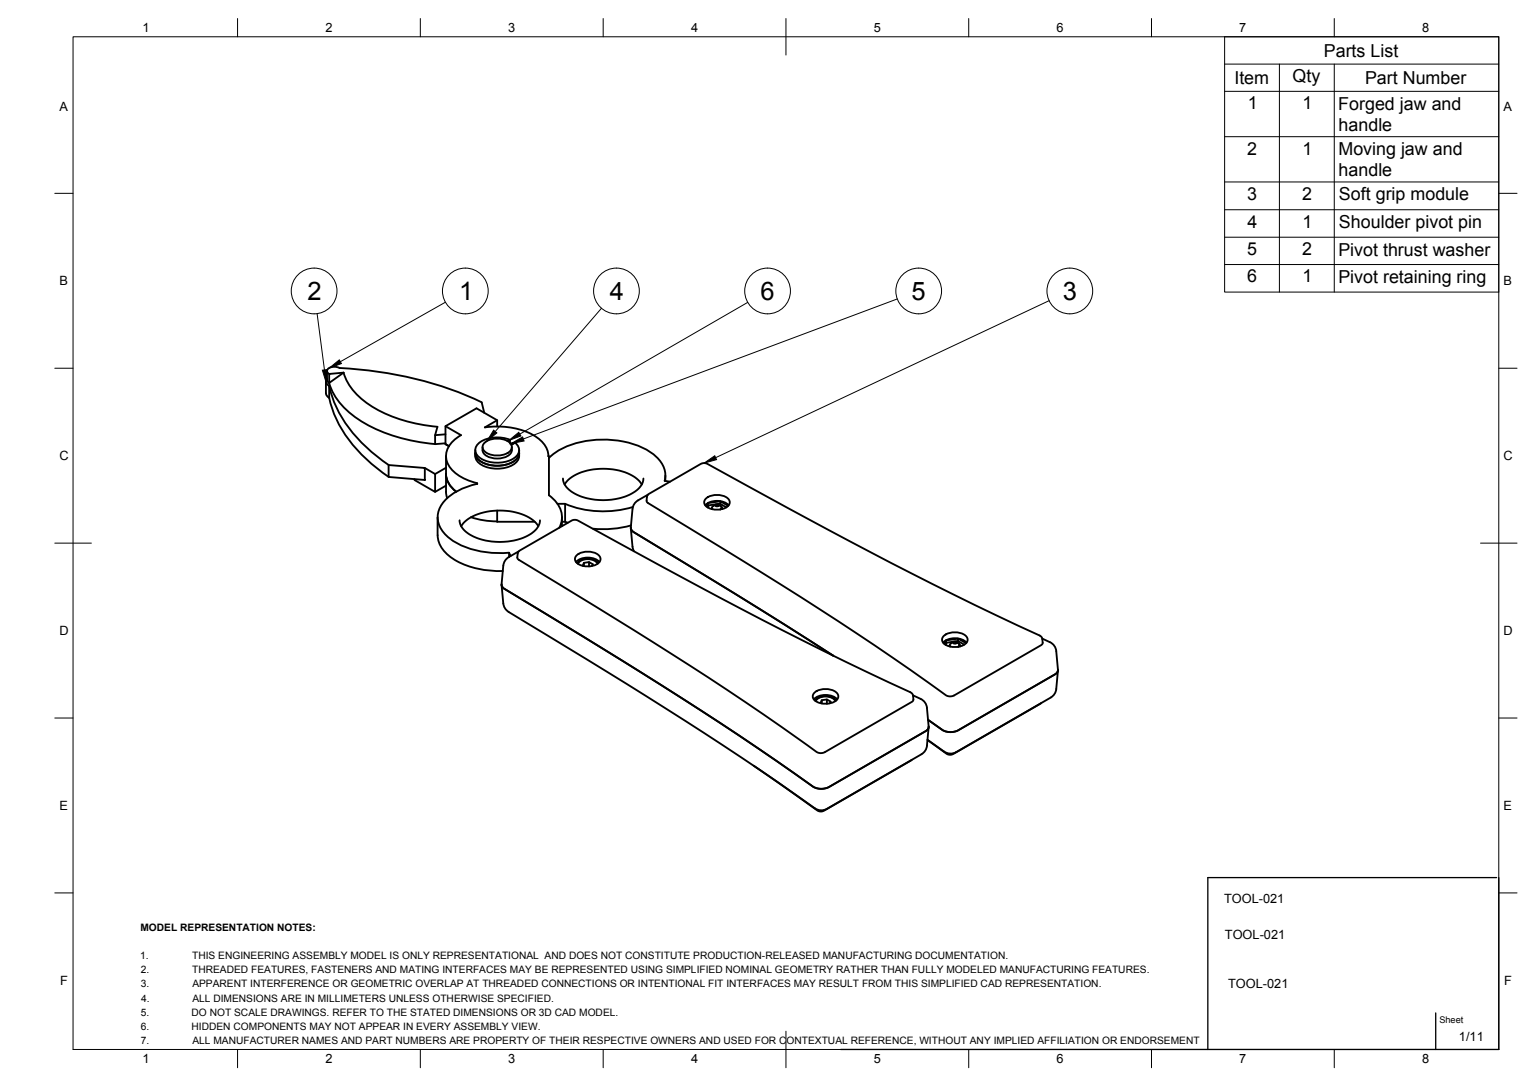
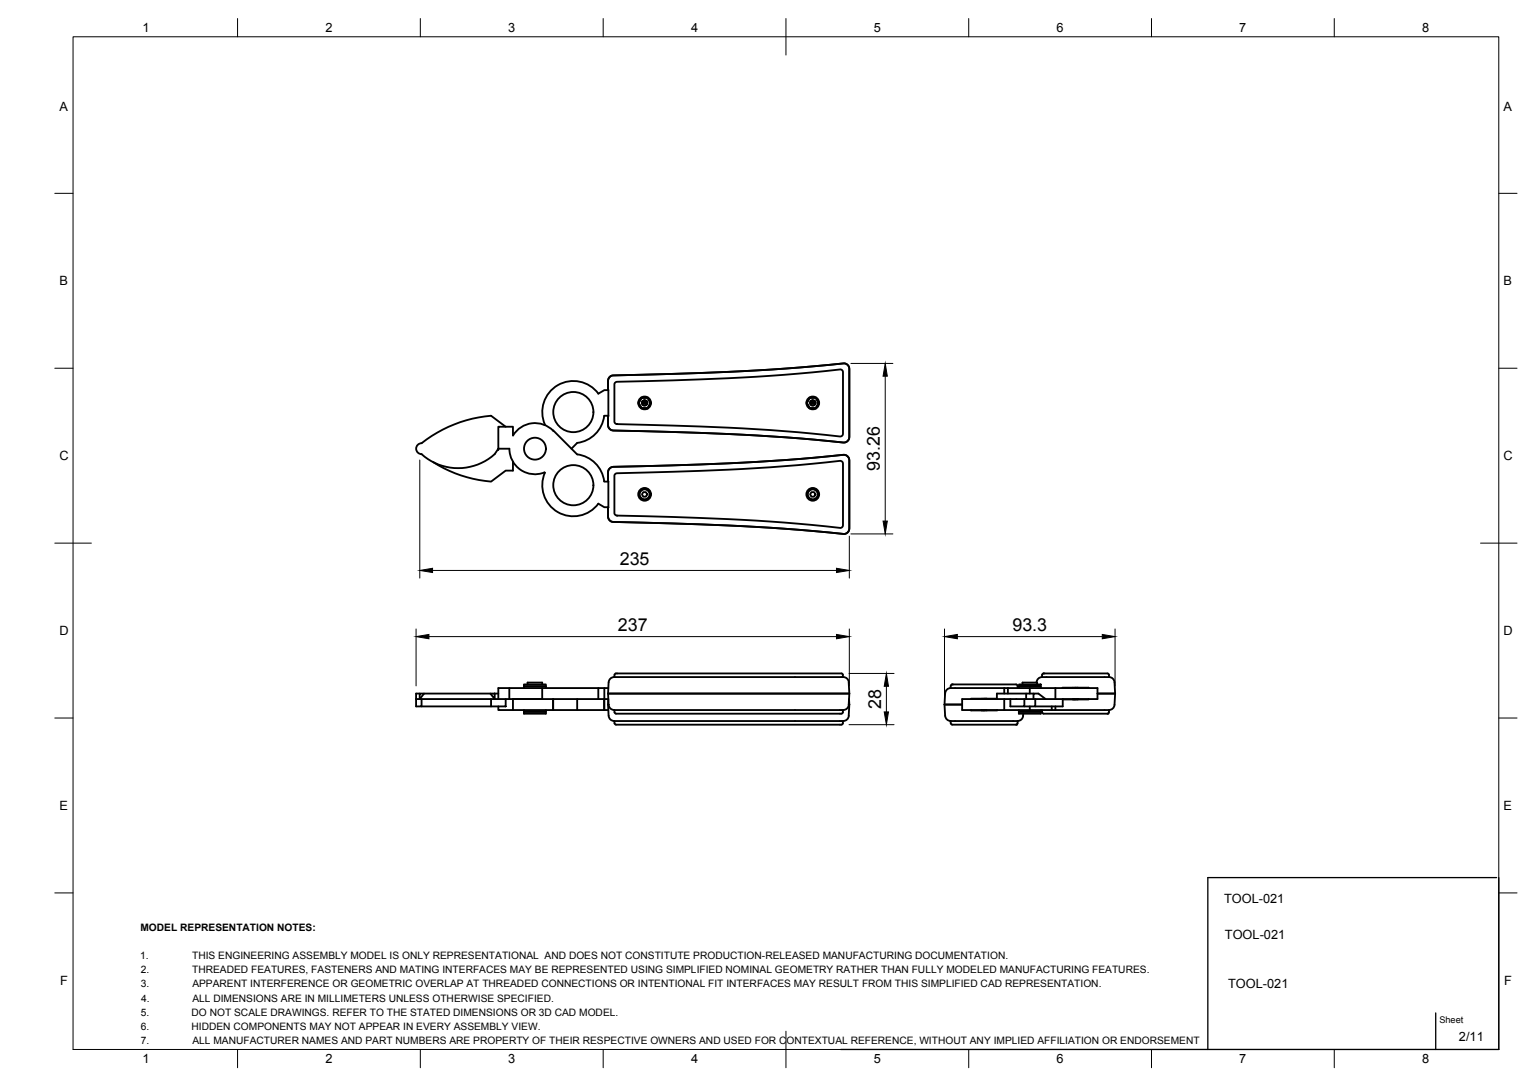
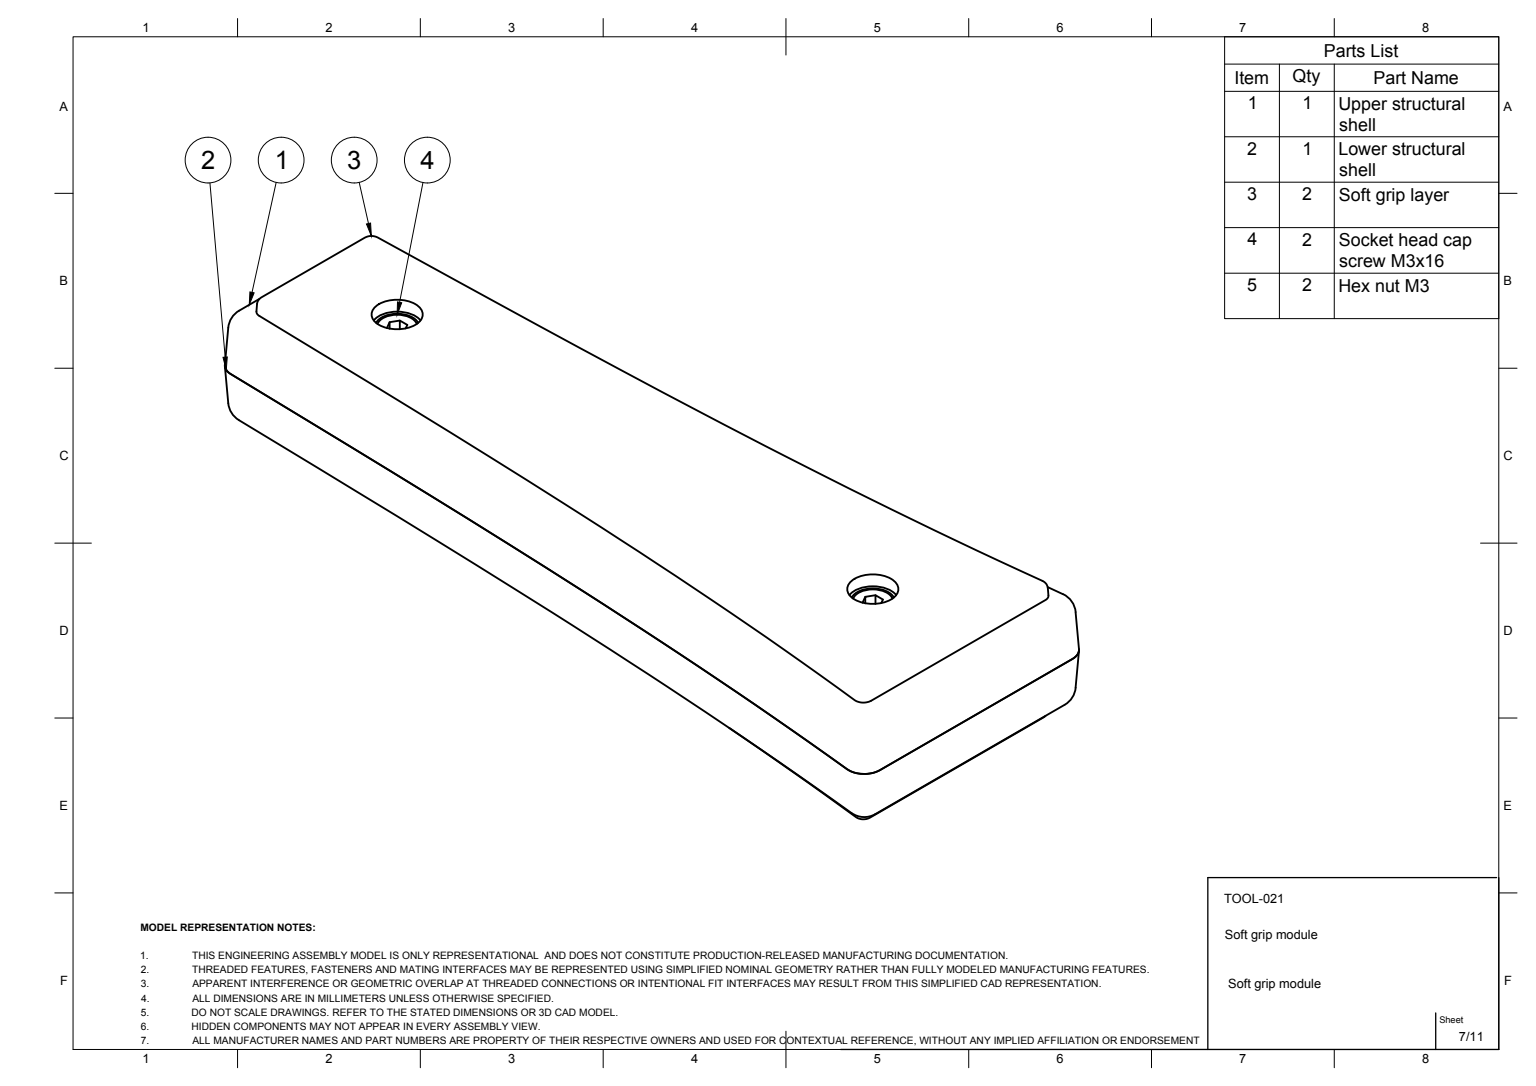
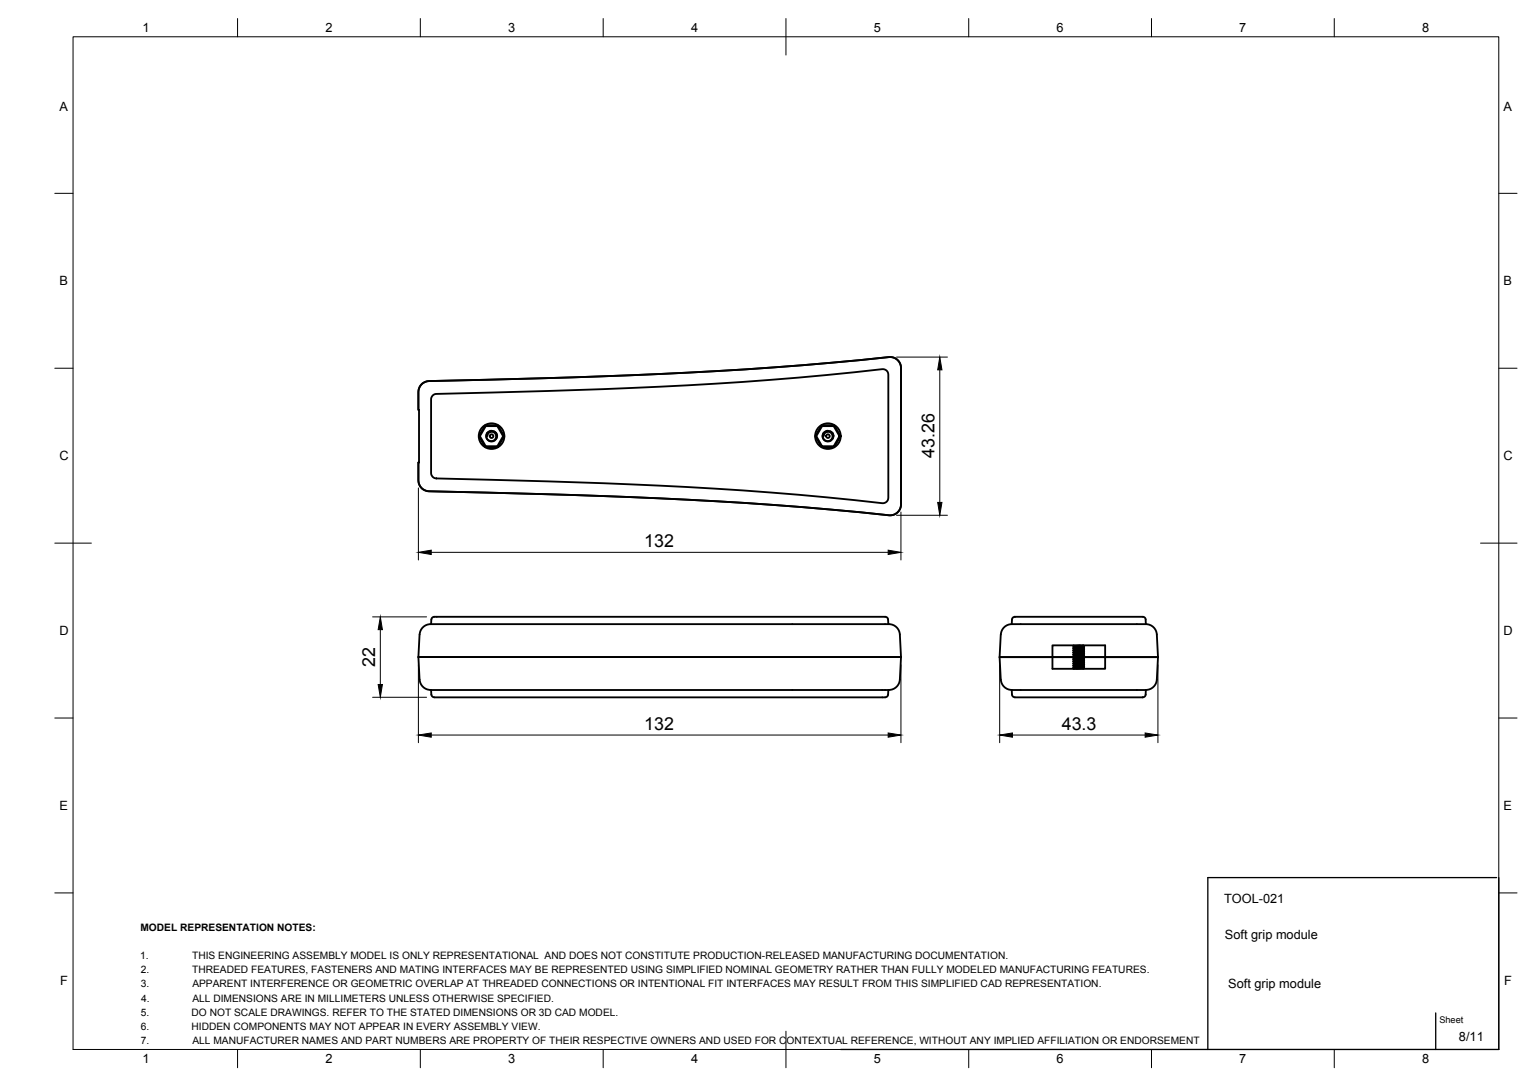
ISO-10303-21;
HEADER;
/* Generated by software containing ST-Developer
 * from STEP Tools, Inc. (www.steptools.com) 
 */

FILE_DESCRIPTION(
/* description */ (''),
/* implementation_level */ '2;1');

FILE_NAME(
/* name */ 'TOOL-021.step',
/* time_stamp */ '2026-11-10T09:05:57-08:00',
/* author */ (''),
/* organization */ (''),
/* preprocessor_version */ 'ST-DEVELOPER v20.2',
/* originating_system */ 'Autodesk Translation Framework v15.17.0.0',
/* authorisation */ '');

FILE_SCHEMA (('AUTOMOTIVE_DESIGN { 1 0 10303 214 3 1 1 }'));
ENDSEC;

DATA;
#10=MECHANICAL_DESIGN_GEOMETRIC_PRESENTATION_REPRESENTATION('',(#565,#566,
#567,#568,#569,#570,#571,#572,#573,#574),#19618);
#11=ITEM_DEFINED_TRANSFORMATION($,$,#7373,#7744);
#12=ITEM_DEFINED_TRANSFORMATION($,$,#7475,#7745);
#13=ITEM_DEFINED_TRANSFORMATION($,$,#7583,#7746);
#14=ITEM_DEFINED_TRANSFORMATION($,$,#7636,#7747);
#15=ITEM_DEFINED_TRANSFORMATION($,$,#7718,#7748);
#16=ITEM_DEFINED_TRANSFORMATION($,$,#7583,#7749);
#17=ITEM_DEFINED_TRANSFORMATION($,$,#7636,#7750);
#18=ITEM_DEFINED_TRANSFORMATION($,$,#7718,#7751);
#19=ITEM_DEFINED_TRANSFORMATION($,$,#7225,#7761);
#20=ITEM_DEFINED_TRANSFORMATION($,$,#7285,#7762);
#21=ITEM_DEFINED_TRANSFORMATION($,$,#7372,#7763);
#22=ITEM_DEFINED_TRANSFORMATION($,$,#7343,#7764);
#23=ITEM_DEFINED_TRANSFORMATION($,$,#7752,#7765);
#24=ITEM_DEFINED_TRANSFORMATION($,$,#7361,#7766);
#25=ITEM_DEFINED_TRANSFORMATION($,$,#7372,#7767);
#26=ITEM_DEFINED_TRANSFORMATION($,$,#7752,#7768);
#27=(
REPRESENTATION_RELATIONSHIP($,$,#19669,#19668)
REPRESENTATION_RELATIONSHIP_WITH_TRANSFORMATION(#11)
SHAPE_REPRESENTATION_RELATIONSHIP()
);
#28=(
REPRESENTATION_RELATIONSHIP($,$,#19670,#19668)
REPRESENTATION_RELATIONSHIP_WITH_TRANSFORMATION(#12)
SHAPE_REPRESENTATION_RELATIONSHIP()
);
#29=(
REPRESENTATION_RELATIONSHIP($,$,#19671,#19668)
REPRESENTATION_RELATIONSHIP_WITH_TRANSFORMATION(#13)
SHAPE_REPRESENTATION_RELATIONSHIP()
);
#30=(
REPRESENTATION_RELATIONSHIP($,$,#19672,#19668)
REPRESENTATION_RELATIONSHIP_WITH_TRANSFORMATION(#14)
SHAPE_REPRESENTATION_RELATIONSHIP()
);
#31=(
REPRESENTATION_RELATIONSHIP($,$,#19673,#19668)
REPRESENTATION_RELATIONSHIP_WITH_TRANSFORMATION(#15)
SHAPE_REPRESENTATION_RELATIONSHIP()
);
#32=(
REPRESENTATION_RELATIONSHIP($,$,#19671,#19668)
REPRESENTATION_RELATIONSHIP_WITH_TRANSFORMATION(#16)
SHAPE_REPRESENTATION_RELATIONSHIP()
);
#33=(
REPRESENTATION_RELATIONSHIP($,$,#19672,#19668)
REPRESENTATION_RELATIONSHIP_WITH_TRANSFORMATION(#17)
SHAPE_REPRESENTATION_RELATIONSHIP()
);
#34=(
REPRESENTATION_RELATIONSHIP($,$,#19673,#19668)
REPRESENTATION_RELATIONSHIP_WITH_TRANSFORMATION(#18)
SHAPE_REPRESENTATION_RELATIONSHIP()
);
#35=(
REPRESENTATION_RELATIONSHIP($,$,#19664,#19663)
REPRESENTATION_RELATIONSHIP_WITH_TRANSFORMATION(#19)
SHAPE_REPRESENTATION_RELATIONSHIP()
);
#36=(
REPRESENTATION_RELATIONSHIP($,$,#19665,#19663)
REPRESENTATION_RELATIONSHIP_WITH_TRANSFORMATION(#20)
SHAPE_REPRESENTATION_RELATIONSHIP()
);
#37=(
REPRESENTATION_RELATIONSHIP($,$,#19668,#19663)
REPRESENTATION_RELATIONSHIP_WITH_TRANSFORMATION(#21)
SHAPE_REPRESENTATION_RELATIONSHIP()
);
#38=(
REPRESENTATION_RELATIONSHIP($,$,#19666,#19663)
REPRESENTATION_RELATIONSHIP_WITH_TRANSFORMATION(#22)
SHAPE_REPRESENTATION_RELATIONSHIP()
);
#39=(
REPRESENTATION_RELATIONSHIP($,$,#19674,#19663)
REPRESENTATION_RELATIONSHIP_WITH_TRANSFORMATION(#23)
SHAPE_REPRESENTATION_RELATIONSHIP()
);
#40=(
REPRESENTATION_RELATIONSHIP($,$,#19667,#19663)
REPRESENTATION_RELATIONSHIP_WITH_TRANSFORMATION(#24)
SHAPE_REPRESENTATION_RELATIONSHIP()
);
#41=(
REPRESENTATION_RELATIONSHIP($,$,#19668,#19663)
REPRESENTATION_RELATIONSHIP_WITH_TRANSFORMATION(#25)
SHAPE_REPRESENTATION_RELATIONSHIP()
);
#42=(
REPRESENTATION_RELATIONSHIP($,$,#19674,#19663)
REPRESENTATION_RELATIONSHIP_WITH_TRANSFORMATION(#26)
SHAPE_REPRESENTATION_RELATIONSHIP()
);
#43=CONTEXT_DEPENDENT_SHAPE_REPRESENTATION(#27,#19646);
#44=CONTEXT_DEPENDENT_SHAPE_REPRESENTATION(#28,#19647);
#45=CONTEXT_DEPENDENT_SHAPE_REPRESENTATION(#29,#19648);
#46=CONTEXT_DEPENDENT_SHAPE_REPRESENTATION(#30,#19649);
#47=CONTEXT_DEPENDENT_SHAPE_REPRESENTATION(#31,#19650);
#48=CONTEXT_DEPENDENT_SHAPE_REPRESENTATION(#32,#19651);
#49=CONTEXT_DEPENDENT_SHAPE_REPRESENTATION(#33,#19652);
#50=CONTEXT_DEPENDENT_SHAPE_REPRESENTATION(#34,#19653);
#51=CONTEXT_DEPENDENT_SHAPE_REPRESENTATION(#35,#19655);
#52=CONTEXT_DEPENDENT_SHAPE_REPRESENTATION(#36,#19656);
#53=CONTEXT_DEPENDENT_SHAPE_REPRESENTATION(#37,#19657);
#54=CONTEXT_DEPENDENT_SHAPE_REPRESENTATION(#38,#19658);
#55=CONTEXT_DEPENDENT_SHAPE_REPRESENTATION(#39,#19659);
#56=CONTEXT_DEPENDENT_SHAPE_REPRESENTATION(#40,#19660);
#57=CONTEXT_DEPENDENT_SHAPE_REPRESENTATION(#41,#19661);
#58=CONTEXT_DEPENDENT_SHAPE_REPRESENTATION(#42,#19662);
#59=NEXT_ASSEMBLY_USAGE_OCCURRENCE('Upper structural shell:1',
'Upper structural shell:1','Upper structural shell:1',#19681,#19682,
'Upper structural shell:1');
#60=NEXT_ASSEMBLY_USAGE_OCCURRENCE('Lower structural shell:1',
'Lower structural shell:1','Lower structural shell:1',#19681,#19683,
'Lower structural shell:1');
#61=NEXT_ASSEMBLY_USAGE_OCCURRENCE('Soft grip layer:1',
'Soft grip layer:1','Soft grip layer:1',#19681,#19684,
'Soft grip layer:1');
#62=NEXT_ASSEMBLY_USAGE_OCCURRENCE('Socket head cap screw M3x16:1',
'Socket head cap screw M3x16:1','Socket head cap screw M3x16:1',#19681,
#19685,'Socket head cap screw M3x16:1');
#63=NEXT_ASSEMBLY_USAGE_OCCURRENCE('Hex nut M3:1','Hex nut M3:1',
'Hex nut M3:1',#19681,#19686,'Hex nut M3:1');
#64=NEXT_ASSEMBLY_USAGE_OCCURRENCE('Soft grip layer:2',
'Soft grip layer:2','Soft grip layer:2',#19681,#19684,
'Soft grip layer:2');
#65=NEXT_ASSEMBLY_USAGE_OCCURRENCE('Socket head cap screw M3x16:2',
'Socket head cap screw M3x16:2','Socket head cap screw M3x16:2',#19681,
#19685,'Socket head cap screw M3x16:2');
#66=NEXT_ASSEMBLY_USAGE_OCCURRENCE('Hex nut M3:2','Hex nut M3:2',
'Hex nut M3:2',#19681,#19686,'Hex nut M3:2');
#67=NEXT_ASSEMBLY_USAGE_OCCURRENCE('Forged jaw and handle:1',
'Forged jaw and handle:1','Forged jaw and handle:1',#19676,#19677,
'Forged jaw and handle:1');
#68=NEXT_ASSEMBLY_USAGE_OCCURRENCE('Moving jaw and handle:1',
'Moving jaw and handle:1','Moving jaw and handle:1',#19676,#19678,
'Moving jaw and handle:1');
#69=NEXT_ASSEMBLY_USAGE_OCCURRENCE('Soft grip module:1',
'Soft grip module:1','Soft grip module:1',#19676,#19681,
'Soft grip module:1');
#70=NEXT_ASSEMBLY_USAGE_OCCURRENCE('Shoulder pivot pin:1',
'Shoulder pivot pin:1','Shoulder pivot pin:1',#19676,#19679,
'Shoulder pivot pin:1');
#71=NEXT_ASSEMBLY_USAGE_OCCURRENCE('Pivot thrust washer:1',
'Pivot thrust washer:1','Pivot thrust washer:1',#19676,#19687,
'Pivot thrust washer:1');
#72=NEXT_ASSEMBLY_USAGE_OCCURRENCE('Pivot retaining ring:1',
'Pivot retaining ring:1','Pivot retaining ring:1',#19676,#19680,
'Pivot retaining ring:1');
#73=NEXT_ASSEMBLY_USAGE_OCCURRENCE('Soft grip module:2',
'Soft grip module:2','Soft grip module:2',#19676,#19681,
'Soft grip module:2');
#74=NEXT_ASSEMBLY_USAGE_OCCURRENCE('Pivot thrust washer:2',
'Pivot thrust washer:2','Pivot thrust washer:2',#19676,#19687,
'Pivot thrust washer:2');
#75=SPHERICAL_SURFACE('',#7438,0.0999999999999999);
#76=SPHERICAL_SURFACE('',#7441,0.0999999999999997);
#77=SPHERICAL_SURFACE('',#7445,0.0999999999999998);
#78=SPHERICAL_SURFACE('',#7449,0.1);
#79=SPHERICAL_SURFACE('',#7454,0.3);
#80=SPHERICAL_SURFACE('',#7458,0.3);
#81=SPHERICAL_SURFACE('',#7462,0.3);
#82=SPHERICAL_SURFACE('',#7467,0.3);
#83=SPHERICAL_SURFACE('',#7546,0.0999999999999999);
#84=SPHERICAL_SURFACE('',#7549,0.0999999999999997);
#85=SPHERICAL_SURFACE('',#7553,0.0999999999999998);
#86=SPHERICAL_SURFACE('',#7557,0.1);
#87=SPHERICAL_SURFACE('',#7562,0.3);
#88=SPHERICAL_SURFACE('',#7566,0.3);
#89=SPHERICAL_SURFACE('',#7570,0.3);
#90=SPHERICAL_SURFACE('',#7575,0.3);
#91=B_SPLINE_SURFACE_WITH_KNOTS('',3,3,((#10711,#10712,#10713,#10714),(#10715,
#10716,#10717,#10718),(#10719,#10720,#10721,#10722),(#10723,#10724,#10725,
#10726)),.UNSPECIFIED.,.F.,.F.,.F.,(4,4),(4,4),(0.0600191787356395,0.326709122771036),
(0.0105314009467253,0.683686938235975),.UNSPECIFIED.);
#92=B_SPLINE_SURFACE_WITH_KNOTS('',3,3,((#10731,#10732,#10733,#10734),(#10735,
#10736,#10737,#10738),(#10739,#10740,#10741,#10742),(#10743,#10744,#10745,
#10746)),.UNSPECIFIED.,.F.,.F.,.F.,(4,4),(4,4),(0.0251675824878611,0.0470055662028096),
(0.0103663370325175,0.682341693918943),.UNSPECIFIED.);
#93=B_SPLINE_SURFACE_WITH_KNOTS('',3,3,((#10756,#10757,#10758,#10759),(#10760,
#10761,#10762,#10763),(#10764,#10765,#10766,#10767),(#10768,#10769,#10770,
#10771),(#10772,#10773,#10774,#10775)),.UNSPECIFIED.,.F.,.F.,.F.,(4,1,4),
(4,4),(0.,0.571428571428571,1.),(0.796205213256333,4.31873271634551),
 .UNSPECIFIED.);
#94=B_SPLINE_SURFACE_WITH_KNOTS('',3,3,((#10780,#10781,#10782,#10783),(#10784,
#10785,#10786,#10787),(#10788,#10789,#10790,#10791),(#10792,#10793,#10794,
#10795),(#10796,#10797,#10798,#10799)),.UNSPECIFIED.,.F.,.F.,.F.,(4,1,4),
(4,4),(0.,0.571428571428571,1.),(0.335767855111383,0.605460332260614),
 .UNSPECIFIED.);
#95=B_SPLINE_SURFACE_WITH_KNOTS('',3,3,((#10818,#10819,#10820,#10821),(#10822,
#10823,#10824,#10825),(#10826,#10827,#10828,#10829),(#10830,#10831,#10832,
#10833),(#10834,#10835,#10836,#10837)),.UNSPECIFIED.,.F.,.F.,.F.,(4,1,4),
(4,4),(0.,0.571428571428571,1.),(8.8675541747208,12.3900816778099),
 .UNSPECIFIED.);
#96=B_SPLINE_SURFACE_WITH_KNOTS('',3,3,((#10842,#10843,#10844,#10845),(#10846,
#10847,#10848,#10849),(#10850,#10851,#10852,#10853),(#10854,#10855,#10856,
#10857)),.UNSPECIFIED.,.F.,.F.,.F.,(4,4),(4,4),(0.673290877228964,0.939980821264432),
(0.010531400969624,0.683686938235975),.UNSPECIFIED.);
#97=B_SPLINE_SURFACE_WITH_KNOTS('',3,3,((#10858,#10859,#10860,#10861),(#10862,
#10863,#10864,#10865),(#10866,#10867,#10868,#10869),(#10870,#10871,#10872,
#10873)),.UNSPECIFIED.,.F.,.F.,.F.,(4,4),(4,4),(0.952994433797115,0.974832417512139),
(0.0103663370325174,0.682341693895801),.UNSPECIFIED.);
#98=B_SPLINE_SURFACE_WITH_KNOTS('',3,3,((#10957,#10958,#10959,#10960),(#10961,
#10962,#10963,#10964),(#10965,#10966,#10967,#10968),(#10969,#10970,#10971,
#10972)),.UNSPECIFIED.,.F.,.F.,.F.,(4,4),(4,4),(0.341076481775573,0.660379921919131),
(0.0113804342297301,0.684288445414502),.UNSPECIFIED.);
#99=B_SPLINE_SURFACE_WITH_KNOTS('',3,3,((#10977,#10978,#10979,#10980),(#10981,
#10982,#10983,#10984),(#10985,#10986,#10987,#10988),(#10989,#10990,#10991,
#10992),(#10993,#10994,#10995,#10996)),.UNSPECIFIED.,.F.,.F.,.F.,(4,1,4),
(4,4),(0.,0.571428571428571,1.),(4.5128966022766,8.72381854299666),
 .UNSPECIFIED.);
#100=B_SPLINE_SURFACE_WITH_KNOTS('',3,3,((#11006,#11007,#11008,#11009),
(#11010,#11011,#11012,#11013),(#11014,#11015,#11016,#11017),(#11018,#11019,
#11020,#11021),(#11022,#11023,#11024,#11025)),.UNSPECIFIED.,.F.,.F.,.F.,
(4,1,4),(4,4),(0.,0.571428571428571,1.),(4.46246834806959,8.67339028878965),
 .UNSPECIFIED.);
#101=B_SPLINE_SURFACE_WITH_KNOTS('',3,3,((#11030,#11031,#11032,#11033),
(#11034,#11035,#11036,#11037),(#11038,#11039,#11040,#11041),(#11042,#11043,
#11044,#11045)),.UNSPECIFIED.,.F.,.F.,.F.,(4,4),(4,4),(0.33962007808087,
0.658923518224427),(0.0113804342297301,0.68428844541339),.UNSPECIFIED.);
#102=B_SPLINE_SURFACE_WITH_KNOTS('',3,3,((#11117,#11118,#11119,#11120),
(#11121,#11122,#11123,#11124),(#11125,#11126,#11127,#11128),(#11129,#11130,
#11131,#11132)),.UNSPECIFIED.,.F.,.F.,.F.,(4,4),(4,4),(0.67474627241906,
0.91907102854965),(0.0117551961069005,0.684448842095107),.UNSPECIFIED.);
#103=B_SPLINE_SURFACE_WITH_KNOTS('',3,3,((#11137,#11138,#11139,#11140),
(#11141,#11142,#11143,#11144),(#11145,#11146,#11147,#11148),(#11149,#11150,
#11151,#11152),(#11153,#11154,#11155,#11156)),.UNSPECIFIED.,.F.,.F.,.F.,
(4,1,4),(4,4),(0.,0.571428571428571,1.),(8.92068531110742,12.1251256661408),
 .UNSPECIFIED.);
#104=B_SPLINE_SURFACE_WITH_KNOTS('',3,3,((#11157,#11158,#11159,#11160),
(#11161,#11162,#11163,#11164),(#11165,#11166,#11167,#11168),(#11169,#11170,
#11171,#11172),(#11173,#11174,#11175,#11176)),.UNSPECIFIED.,.F.,.F.,.F.,
(4,1,4),(4,4),(0.,0.571428571428571,1.),(1.06116122492545,4.26560157995882),
 .UNSPECIFIED.);
#105=B_SPLINE_SURFACE_WITH_KNOTS('',3,3,((#11181,#11182,#11183,#11184),
(#11185,#11186,#11187,#11188),(#11189,#11190,#11191,#11192),(#11193,#11194,
#11195,#11196)),.UNSPECIFIED.,.F.,.F.,.F.,(4,4),(4,4),(0.0809289714503497,
0.325253727580939),(0.011755196108102,0.684448842095106),.UNSPECIFIED.);
#106=B_SPLINE_SURFACE_WITH_KNOTS('',3,3,((#11271,#11272,#11273,#11274),
(#11275,#11276,#11277,#11278),(#11279,#11280,#11281,#11282),(#11283,#11284,
#11285,#11286)),.UNSPECIFIED.,.F.,.F.,.F.,(4,4),(4,4),(0.932204931312898,
0.977820042778932),(0.0118590921259657,0.68448768567755),.UNSPECIFIED.);
#107=B_SPLINE_SURFACE_WITH_KNOTS('',3,3,((#11296,#11297,#11298,#11299),
(#11300,#11301,#11302,#11303),(#11304,#11305,#11306,#11307),(#11308,#11309,
#11310,#11311),(#11312,#11313,#11314,#11315)),.UNSPECIFIED.,.F.,.F.,.F.,
(4,1,4),(4,4),(0.,0.571428571428571,1.),(12.3228618033436,12.893479658151),
 .UNSPECIFIED.);
#108=B_SPLINE_SURFACE_WITH_KNOTS('',3,3,((#11329,#11330,#11331,#11332),
(#11333,#11334,#11335,#11336),(#11337,#11338,#11339,#11340),(#11341,#11342,
#11343,#11344)),.UNSPECIFIED.,.F.,.F.,.F.,(4,4),(4,4),(0.0221799572210682,
0.0677950686870383),(0.0118590921467069,0.68448768567755),.UNSPECIFIED.);
#109=B_SPLINE_SURFACE_WITH_KNOTS('',3,3,((#11354,#11355,#11356,#11357),
(#11358,#11359,#11360,#11361),(#11362,#11363,#11364,#11365),(#11366,#11367,
#11368,#11369),(#11370,#11371,#11372,#11373)),.UNSPECIFIED.,.F.,.F.,.F.,
(4,1,4),(4,4),(0.,0.571428571428571,1.),(0.29280723291527,0.863425087722636),
 .UNSPECIFIED.);
#110=B_SPLINE_SURFACE_WITH_KNOTS('',3,3,((#11387,#11388,#11389,#11390),
(#11391,#11392,#11393,#11394),(#11395,#11396,#11397,#11398),(#11399,#11400,
#11401,#11402),(#11403,#11404,#11405,#11406)),.UNSPECIFIED.,.F.,.F.,.F.,
(4,1,4),(4,4),(0.,0.571428571428571,1.),(0.00866835330220971,0.617725317592517),
 .UNSPECIFIED.);
#111=B_SPLINE_SURFACE_WITH_KNOTS('',3,3,((#11413,#11414,#11415,#11416),
(#11417,#11418,#11419,#11420),(#11421,#11422,#11423,#11424),(#11425,#11426,
#11427,#11428),(#11429,#11430,#11431,#11432),(#11433,#11434,#11435,#11436)),
 .UNSPECIFIED.,.F.,.F.,.F.,(4,1,1,4),(4,4),(0.,0.285714285714286,0.571428571428571,
1.),(0.00654045782928703,0.615688454110788),.UNSPECIFIED.);
#112=B_SPLINE_SURFACE_WITH_KNOTS('',3,3,((#11441,#11442,#11443,#11444),
(#11445,#11446,#11447,#11448),(#11449,#11450,#11451,#11452),(#11453,#11454,
#11455,#11456),(#11457,#11458,#11459,#11460),(#11461,#11462,#11463,#11464)),
 .UNSPECIFIED.,.F.,.F.,.F.,(4,1,1,4),(4,4),(0.,0.285714285714286,0.571428571428571,
1.),(0.00659363931523289,0.615688454110787),.UNSPECIFIED.);
#113=B_SPLINE_SURFACE_WITH_KNOTS('',3,3,((#11469,#11470,#11471,#11472),
(#11473,#11474,#11475,#11476),(#11477,#11478,#11479,#11480),(#11481,#11482,
#11483,#11484),(#11485,#11486,#11487,#11488)),.UNSPECIFIED.,.F.,.F.,.F.,
(4,1,4),(4,4),(0.,0.571428571428571,1.),(12.5808265588057,12.8505190359549),
 .UNSPECIFIED.);
#114=B_SPLINE_SURFACE_WITH_KNOTS('',3,3,((#11489,#11490,#11491,#11492),
(#11493,#11494,#11495,#11496),(#11497,#11498,#11499,#11500),(#11501,#11502,
#11503,#11504),(#11505,#11506,#11507,#11508)),.UNSPECIFIED.,.F.,.F.,.F.,
(4,1,4),(4,4),(0.,0.571428571428571,1.),(0.00865878607617127,0.617725317592517),
 .UNSPECIFIED.);
#115=B_SPLINE_SURFACE_WITH_KNOTS('',3,3,((#11534,#11535,#11536,#11537),
(#11538,#11539,#11540,#11541),(#11542,#11543,#11544,#11545),(#11546,#11547,
#11548,#11549),(#11550,#11551,#11552,#11553)),.UNSPECIFIED.,.F.,.F.,.F.,
(4,1,4),(4,4),(0.,0.571428571428571,1.),(-0.00615755989250974,0.617725317592517),
 .UNSPECIFIED.);
#116=B_SPLINE_SURFACE_WITH_KNOTS('',3,3,((#11572,#11573,#11574,#11575,#11576),
(#11577,#11578,#11579,#11580,#11581),(#11582,#11583,#11584,#11585,#11586),
(#11587,#11588,#11589,#11590,#11591),(#11592,#11593,#11594,#11595,#11596)),
 .UNSPECIFIED.,.F.,.F.,.F.,(4,1,4),(4,1,4),(0.,0.571428571428571,1.),(0.335767855111383,
5.71764434212835,12.893479658151),.UNSPECIFIED.);
#117=B_SPLINE_SURFACE_WITH_KNOTS('',3,3,((#11607,#11608,#11609,#11610),
(#11611,#11612,#11613,#11614),(#11615,#11616,#11617,#11618),(#11619,#11620,
#11621,#11622),(#11623,#11624,#11625,#11626),(#11627,#11628,#11629,#11630)),
 .UNSPECIFIED.,.F.,.F.,.F.,(4,1,1,4),(4,4),(0.,0.285714285714286,0.571428571428571,
1.),(-0.00844595120920508,0.615688454110788),.UNSPECIFIED.);
#118=B_SPLINE_SURFACE_WITH_KNOTS('',3,3,((#11639,#11640,#11641,#11642),
(#11643,#11644,#11645,#11646),(#11647,#11648,#11649,#11650),(#11651,#11652,
#11653,#11654),(#11655,#11656,#11657,#11658),(#11659,#11660,#11661,#11662)),
 .UNSPECIFIED.,.F.,.F.,.F.,(4,1,1,4),(4,4),(0.,0.285714285714286,0.571428571428571,
1.),(-0.00828643285111643,0.615688454110787),.UNSPECIFIED.);
#119=B_SPLINE_SURFACE_WITH_KNOTS('',3,3,((#11671,#11672,#11673,#11674,#11675),
(#11676,#11677,#11678,#11679,#11680),(#11681,#11682,#11683,#11684,#11685),
(#11686,#11687,#11688,#11689,#11690),(#11691,#11692,#11693,#11694,#11695)),
 .UNSPECIFIED.,.F.,.F.,.F.,(4,1,4),(4,1,4),(0.,0.571428571428571,1.),(0.29280723291527,
7.4686425489379,12.8505190359549),.UNSPECIFIED.);
#120=B_SPLINE_SURFACE_WITH_KNOTS('',3,3,((#11706,#11707,#11708,#11709),
(#11710,#11711,#11712,#11713),(#11714,#11715,#11716,#11717),(#11718,#11719,
#11720,#11721),(#11722,#11723,#11724,#11725)),.UNSPECIFIED.,.F.,.F.,.F.,
(4,1,4),(4,4),(0.,0.571428571428571,1.),(-0.0061862132014275,0.617725317592517),
 .UNSPECIFIED.);
#121=B_SPLINE_SURFACE_WITH_KNOTS('',3,3,((#11734,#11735,#11736,#11737),
(#11738,#11739,#11740,#11741),(#11742,#11743,#11744,#11745),(#11746,#11747,
#11748,#11749)),.UNSPECIFIED.,.F.,.F.,.F.,(4,4),(4,4),(0.025165545222094,
0.977821881680028),(0.,0.68448768567755),.UNSPECIFIED.);
#122=B_SPLINE_SURFACE_WITH_KNOTS('',3,3,((#11752,#11753,#11754,#11755),
(#11756,#11757,#11758,#11759),(#11760,#11761,#11762,#11763),(#11764,#11765,
#11766,#11767)),.UNSPECIFIED.,.F.,.F.,.F.,(4,4),(4,4),(0.0221781183199723,
0.974834454777906),(0.,0.68448768567755),.UNSPECIFIED.);
#123=B_SPLINE_SURFACE_WITH_KNOTS('',3,3,((#12819,#12820,#12821,#12822),
(#12823,#12824,#12825,#12826),(#12827,#12828,#12829,#12830),(#12831,#12832,
#12833,#12834)),.UNSPECIFIED.,.F.,.F.,.F.,(4,4),(4,4),(0.0600191787356395,
0.326709122771036),(0.0105314009467253,0.683686938235975),.UNSPECIFIED.);
#124=B_SPLINE_SURFACE_WITH_KNOTS('',3,3,((#12839,#12840,#12841,#12842),
(#12843,#12844,#12845,#12846),(#12847,#12848,#12849,#12850),(#12851,#12852,
#12853,#12854)),.UNSPECIFIED.,.F.,.F.,.F.,(4,4),(4,4),(0.0251675824878611,
0.0470055662028096),(0.0103663370325175,0.682341693918943),
 .UNSPECIFIED.);
#125=B_SPLINE_SURFACE_WITH_KNOTS('',3,3,((#12864,#12865,#12866,#12867),
(#12868,#12869,#12870,#12871),(#12872,#12873,#12874,#12875),(#12876,#12877,
#12878,#12879),(#12880,#12881,#12882,#12883)),.UNSPECIFIED.,.F.,.F.,.F.,
(4,1,4),(4,4),(0.,0.571428571428571,1.),(0.796205213256333,4.31873271634551),
 .UNSPECIFIED.);
#126=B_SPLINE_SURFACE_WITH_KNOTS('',3,3,((#12888,#12889,#12890,#12891),
(#12892,#12893,#12894,#12895),(#12896,#12897,#12898,#12899),(#12900,#12901,
#12902,#12903),(#12904,#12905,#12906,#12907)),.UNSPECIFIED.,.F.,.F.,.F.,
(4,1,4),(4,4),(0.,0.571428571428571,1.),(0.335767855111383,0.605460332260614),
 .UNSPECIFIED.);
#127=B_SPLINE_SURFACE_WITH_KNOTS('',3,3,((#12926,#12927,#12928,#12929),
(#12930,#12931,#12932,#12933),(#12934,#12935,#12936,#12937),(#12938,#12939,
#12940,#12941),(#12942,#12943,#12944,#12945)),.UNSPECIFIED.,.F.,.F.,.F.,
(4,1,4),(4,4),(0.,0.571428571428571,1.),(8.8675541747208,12.3900816778099),
 .UNSPECIFIED.);
#128=B_SPLINE_SURFACE_WITH_KNOTS('',3,3,((#12950,#12951,#12952,#12953),
(#12954,#12955,#12956,#12957),(#12958,#12959,#12960,#12961),(#12962,#12963,
#12964,#12965)),.UNSPECIFIED.,.F.,.F.,.F.,(4,4),(4,4),(0.673290877228964,
0.939980821264432),(0.010531400969624,0.683686938235975),.UNSPECIFIED.);
#129=B_SPLINE_SURFACE_WITH_KNOTS('',3,3,((#12966,#12967,#12968,#12969),
(#12970,#12971,#12972,#12973),(#12974,#12975,#12976,#12977),(#12978,#12979,
#12980,#12981)),.UNSPECIFIED.,.F.,.F.,.F.,(4,4),(4,4),(0.952994433797115,
0.974832417512139),(0.0103663370325174,0.682341693895801),.UNSPECIFIED.);
#130=B_SPLINE_SURFACE_WITH_KNOTS('',3,3,((#13065,#13066,#13067,#13068),
(#13069,#13070,#13071,#13072),(#13073,#13074,#13075,#13076),(#13077,#13078,
#13079,#13080)),.UNSPECIFIED.,.F.,.F.,.F.,(4,4),(4,4),(0.341076481775573,
0.660379921919131),(0.0113804342297301,0.684288445414502),.UNSPECIFIED.);
#131=B_SPLINE_SURFACE_WITH_KNOTS('',3,3,((#13085,#13086,#13087,#13088),
(#13089,#13090,#13091,#13092),(#13093,#13094,#13095,#13096),(#13097,#13098,
#13099,#13100),(#13101,#13102,#13103,#13104)),.UNSPECIFIED.,.F.,.F.,.F.,
(4,1,4),(4,4),(0.,0.571428571428571,1.),(4.5128966022766,8.72381854299666),
 .UNSPECIFIED.);
#132=B_SPLINE_SURFACE_WITH_KNOTS('',3,3,((#13114,#13115,#13116,#13117),
(#13118,#13119,#13120,#13121),(#13122,#13123,#13124,#13125),(#13126,#13127,
#13128,#13129),(#13130,#13131,#13132,#13133)),.UNSPECIFIED.,.F.,.F.,.F.,
(4,1,4),(4,4),(0.,0.571428571428571,1.),(4.46246834806959,8.67339028878965),
 .UNSPECIFIED.);
#133=B_SPLINE_SURFACE_WITH_KNOTS('',3,3,((#13138,#13139,#13140,#13141),
(#13142,#13143,#13144,#13145),(#13146,#13147,#13148,#13149),(#13150,#13151,
#13152,#13153)),.UNSPECIFIED.,.F.,.F.,.F.,(4,4),(4,4),(0.33962007808087,
0.658923518224427),(0.0113804342297301,0.68428844541339),.UNSPECIFIED.);
#134=B_SPLINE_SURFACE_WITH_KNOTS('',3,3,((#13225,#13226,#13227,#13228),
(#13229,#13230,#13231,#13232),(#13233,#13234,#13235,#13236),(#13237,#13238,
#13239,#13240)),.UNSPECIFIED.,.F.,.F.,.F.,(4,4),(4,4),(0.67474627241906,
0.91907102854965),(0.0117551961069005,0.684448842095107),.UNSPECIFIED.);
#135=B_SPLINE_SURFACE_WITH_KNOTS('',3,3,((#13245,#13246,#13247,#13248),
(#13249,#13250,#13251,#13252),(#13253,#13254,#13255,#13256),(#13257,#13258,
#13259,#13260),(#13261,#13262,#13263,#13264)),.UNSPECIFIED.,.F.,.F.,.F.,
(4,1,4),(4,4),(0.,0.571428571428571,1.),(8.92068531110742,12.1251256661408),
 .UNSPECIFIED.);
#136=B_SPLINE_SURFACE_WITH_KNOTS('',3,3,((#13265,#13266,#13267,#13268),
(#13269,#13270,#13271,#13272),(#13273,#13274,#13275,#13276),(#13277,#13278,
#13279,#13280),(#13281,#13282,#13283,#13284)),.UNSPECIFIED.,.F.,.F.,.F.,
(4,1,4),(4,4),(0.,0.571428571428571,1.),(1.06116122492545,4.26560157995882),
 .UNSPECIFIED.);
#137=B_SPLINE_SURFACE_WITH_KNOTS('',3,3,((#13289,#13290,#13291,#13292),
(#13293,#13294,#13295,#13296),(#13297,#13298,#13299,#13300),(#13301,#13302,
#13303,#13304)),.UNSPECIFIED.,.F.,.F.,.F.,(4,4),(4,4),(0.0809289714503497,
0.325253727580939),(0.011755196108102,0.684448842095106),.UNSPECIFIED.);
#138=B_SPLINE_SURFACE_WITH_KNOTS('',3,3,((#13379,#13380,#13381,#13382),
(#13383,#13384,#13385,#13386),(#13387,#13388,#13389,#13390),(#13391,#13392,
#13393,#13394)),.UNSPECIFIED.,.F.,.F.,.F.,(4,4),(4,4),(0.932204931312898,
0.977820042778932),(0.0118590921259657,0.68448768567755),.UNSPECIFIED.);
#139=B_SPLINE_SURFACE_WITH_KNOTS('',3,3,((#13404,#13405,#13406,#13407),
(#13408,#13409,#13410,#13411),(#13412,#13413,#13414,#13415),(#13416,#13417,
#13418,#13419),(#13420,#13421,#13422,#13423)),.UNSPECIFIED.,.F.,.F.,.F.,
(4,1,4),(4,4),(0.,0.571428571428571,1.),(12.3228618033436,12.893479658151),
 .UNSPECIFIED.);
#140=B_SPLINE_SURFACE_WITH_KNOTS('',3,3,((#13437,#13438,#13439,#13440),
(#13441,#13442,#13443,#13444),(#13445,#13446,#13447,#13448),(#13449,#13450,
#13451,#13452)),.UNSPECIFIED.,.F.,.F.,.F.,(4,4),(4,4),(0.0221799572210682,
0.0677950686870383),(0.0118590921467069,0.68448768567755),.UNSPECIFIED.);
#141=B_SPLINE_SURFACE_WITH_KNOTS('',3,3,((#13462,#13463,#13464,#13465),
(#13466,#13467,#13468,#13469),(#13470,#13471,#13472,#13473),(#13474,#13475,
#13476,#13477),(#13478,#13479,#13480,#13481)),.UNSPECIFIED.,.F.,.F.,.F.,
(4,1,4),(4,4),(0.,0.571428571428571,1.),(0.29280723291527,0.863425087722636),
 .UNSPECIFIED.);
#142=B_SPLINE_SURFACE_WITH_KNOTS('',3,3,((#13495,#13496,#13497,#13498),
(#13499,#13500,#13501,#13502),(#13503,#13504,#13505,#13506),(#13507,#13508,
#13509,#13510),(#13511,#13512,#13513,#13514)),.UNSPECIFIED.,.F.,.F.,.F.,
(4,1,4),(4,4),(0.,0.571428571428571,1.),(0.00866835330220971,0.617725317592517),
 .UNSPECIFIED.);
#143=B_SPLINE_SURFACE_WITH_KNOTS('',3,3,((#13521,#13522,#13523,#13524),
(#13525,#13526,#13527,#13528),(#13529,#13530,#13531,#13532),(#13533,#13534,
#13535,#13536),(#13537,#13538,#13539,#13540),(#13541,#13542,#13543,#13544)),
 .UNSPECIFIED.,.F.,.F.,.F.,(4,1,1,4),(4,4),(0.,0.285714285714286,0.571428571428571,
1.),(0.00654045782928703,0.615688454110788),.UNSPECIFIED.);
#144=B_SPLINE_SURFACE_WITH_KNOTS('',3,3,((#13549,#13550,#13551,#13552),
(#13553,#13554,#13555,#13556),(#13557,#13558,#13559,#13560),(#13561,#13562,
#13563,#13564),(#13565,#13566,#13567,#13568),(#13569,#13570,#13571,#13572)),
 .UNSPECIFIED.,.F.,.F.,.F.,(4,1,1,4),(4,4),(0.,0.285714285714286,0.571428571428571,
1.),(0.00659363931523289,0.615688454110787),.UNSPECIFIED.);
#145=B_SPLINE_SURFACE_WITH_KNOTS('',3,3,((#13577,#13578,#13579,#13580),
(#13581,#13582,#13583,#13584),(#13585,#13586,#13587,#13588),(#13589,#13590,
#13591,#13592),(#13593,#13594,#13595,#13596)),.UNSPECIFIED.,.F.,.F.,.F.,
(4,1,4),(4,4),(0.,0.571428571428571,1.),(12.5808265588057,12.8505190359549),
 .UNSPECIFIED.);
#146=B_SPLINE_SURFACE_WITH_KNOTS('',3,3,((#13597,#13598,#13599,#13600),
(#13601,#13602,#13603,#13604),(#13605,#13606,#13607,#13608),(#13609,#13610,
#13611,#13612),(#13613,#13614,#13615,#13616)),.UNSPECIFIED.,.F.,.F.,.F.,
(4,1,4),(4,4),(0.,0.571428571428571,1.),(0.00865878607617127,0.617725317592517),
 .UNSPECIFIED.);
#147=B_SPLINE_SURFACE_WITH_KNOTS('',3,3,((#13642,#13643,#13644,#13645),
(#13646,#13647,#13648,#13649),(#13650,#13651,#13652,#13653),(#13654,#13655,
#13656,#13657),(#13658,#13659,#13660,#13661)),.UNSPECIFIED.,.F.,.F.,.F.,
(4,1,4),(4,4),(0.,0.571428571428571,1.),(-0.00615755989250974,0.617725317592517),
 .UNSPECIFIED.);
#148=B_SPLINE_SURFACE_WITH_KNOTS('',3,3,((#13680,#13681,#13682,#13683,#13684),
(#13685,#13686,#13687,#13688,#13689),(#13690,#13691,#13692,#13693,#13694),
(#13695,#13696,#13697,#13698,#13699),(#13700,#13701,#13702,#13703,#13704)),
 .UNSPECIFIED.,.F.,.F.,.F.,(4,1,4),(4,1,4),(0.,0.571428571428571,1.),(0.335767855111383,
5.71764434212835,12.893479658151),.UNSPECIFIED.);
#149=B_SPLINE_SURFACE_WITH_KNOTS('',3,3,((#13715,#13716,#13717,#13718),
(#13719,#13720,#13721,#13722),(#13723,#13724,#13725,#13726),(#13727,#13728,
#13729,#13730),(#13731,#13732,#13733,#13734),(#13735,#13736,#13737,#13738)),
 .UNSPECIFIED.,.F.,.F.,.F.,(4,1,1,4),(4,4),(0.,0.285714285714286,0.571428571428571,
1.),(-0.00844595120920508,0.615688454110788),.UNSPECIFIED.);
#150=B_SPLINE_SURFACE_WITH_KNOTS('',3,3,((#13747,#13748,#13749,#13750),
(#13751,#13752,#13753,#13754),(#13755,#13756,#13757,#13758),(#13759,#13760,
#13761,#13762),(#13763,#13764,#13765,#13766),(#13767,#13768,#13769,#13770)),
 .UNSPECIFIED.,.F.,.F.,.F.,(4,1,1,4),(4,4),(0.,0.285714285714286,0.571428571428571,
1.),(-0.00828643285111643,0.615688454110787),.UNSPECIFIED.);
#151=B_SPLINE_SURFACE_WITH_KNOTS('',3,3,((#13779,#13780,#13781,#13782,#13783),
(#13784,#13785,#13786,#13787,#13788),(#13789,#13790,#13791,#13792,#13793),
(#13794,#13795,#13796,#13797,#13798),(#13799,#13800,#13801,#13802,#13803)),
 .UNSPECIFIED.,.F.,.F.,.F.,(4,1,4),(4,1,4),(0.,0.571428571428571,1.),(0.29280723291527,
7.4686425489379,12.8505190359549),.UNSPECIFIED.);
#152=B_SPLINE_SURFACE_WITH_KNOTS('',3,3,((#13814,#13815,#13816,#13817),
(#13818,#13819,#13820,#13821),(#13822,#13823,#13824,#13825),(#13826,#13827,
#13828,#13829),(#13830,#13831,#13832,#13833)),.UNSPECIFIED.,.F.,.F.,.F.,
(4,1,4),(4,4),(0.,0.571428571428571,1.),(-0.0061862132014275,0.617725317592517),
 .UNSPECIFIED.);
#153=B_SPLINE_SURFACE_WITH_KNOTS('',3,3,((#13842,#13843,#13844,#13845),
(#13846,#13847,#13848,#13849),(#13850,#13851,#13852,#13853),(#13854,#13855,
#13856,#13857)),.UNSPECIFIED.,.F.,.F.,.F.,(4,4),(4,4),(0.025165545222094,
0.977821881680028),(0.,0.68448768567755),.UNSPECIFIED.);
#154=B_SPLINE_SURFACE_WITH_KNOTS('',3,3,((#13860,#13861,#13862,#13863),
(#13864,#13865,#13866,#13867),(#13868,#13869,#13870,#13871),(#13872,#13873,
#13874,#13875)),.UNSPECIFIED.,.F.,.F.,.F.,(4,4),(4,4),(0.0221781183199723,
0.974834454777906),(0.,0.68448768567755),.UNSPECIFIED.);
#155=B_SPLINE_SURFACE_WITH_KNOTS('',3,3,((#13946,#13947,#13948,#13949,#13950),
(#13951,#13952,#13953,#13954,#13955),(#13956,#13957,#13958,#13959,#13960),
(#13961,#13962,#13963,#13964,#13965),(#13966,#13967,#13968,#13969,#13970)),
 .UNSPECIFIED.,.F.,.F.,.F.,(4,1,4),(4,1,4),(0.,0.571428571428571,1.),(0.,
0.0505788685273923,0.118017359897249),.UNSPECIFIED.);
#156=B_SPLINE_SURFACE_WITH_KNOTS('',3,3,((#13993,#13994,#13995,#13996,#13997),
(#13998,#13999,#14000,#14001,#14002),(#14003,#14004,#14005,#14006,#14007),
(#14008,#14009,#14010,#14011,#14012),(#14013,#14014,#14015,#14016,#14017)),
 .UNSPECIFIED.,.F.,.F.,.F.,(4,1,4),(4,1,4),(0.,0.571428571428571,1.),(0.,
0.0505788685278266,0.118017359898262),.UNSPECIFIED.);
#157=B_SPLINE_SURFACE_WITH_KNOTS('',3,3,((#14031,#14032,#14033,#14034,#14035),
(#14036,#14037,#14038,#14039,#14040),(#14041,#14042,#14043,#14044,#14045),
(#14046,#14047,#14048,#14049,#14050),(#14051,#14052,#14053,#14054,#14055)),
 .UNSPECIFIED.,.F.,.F.,.F.,(4,1,4),(4,1,4),(0.,0.571428571428571,1.),(0.,
5.23288834931112,12.2100728150593),.UNSPECIFIED.);
#158=B_SPLINE_SURFACE_WITH_KNOTS('',3,3,((#14069,#14070,#14071,#14072,#14073),
(#14074,#14075,#14076,#14077,#14078),(#14079,#14080,#14081,#14082,#14083),
(#14084,#14085,#14086,#14087,#14088),(#14089,#14090,#14091,#14092,#14093)),
 .UNSPECIFIED.,.F.,.F.,.F.,(4,1,4),(4,1,4),(0.,0.571428571428571,1.),(1.97133828064127E-11,
0.0463413823988794,0.108129892237767),.UNSPECIFIED.);
#159=B_SPLINE_SURFACE_WITH_KNOTS('',3,3,((#14113,#14114,#14115,#14116,#14117),
(#14118,#14119,#14120,#14121,#14122),(#14123,#14124,#14125,#14126,#14127),
(#14128,#14129,#14130,#14131,#14132),(#14133,#14134,#14135,#14136,#14137)),
 .UNSPECIFIED.,.F.,.F.,.F.,(4,1,4),(4,1,4),(0.,0.571428571428571,1.),(0.,
0.0463413823743492,0.108129892206815),.UNSPECIFIED.);
#160=B_SPLINE_SURFACE_WITH_KNOTS('',3,3,((#14151,#14152,#14153,#14154,#14155),
(#14156,#14157,#14158,#14159,#14160),(#14161,#14162,#14163,#14164,#14165),
(#14166,#14167,#14168,#14169,#14170),(#14171,#14172,#14173,#14174,#14175)),
 .UNSPECIFIED.,.F.,.F.,.F.,(4,1,4),(4,1,4),(0.,0.571428571428571,1.),(6.51086303075479E-13,
6.97718480957529,12.2100734167563),.UNSPECIFIED.);
#161=B_SPLINE_SURFACE_WITH_KNOTS('',3,3,((#14198,#14199,#14200,#14201),
(#14202,#14203,#14204,#14205),(#14206,#14207,#14208,#14209),(#14210,#14211,
#14212,#14213),(#14214,#14215,#14216,#14217)),.UNSPECIFIED.,.F.,.F.,.F.,
(4,1,4),(4,4),(0.,0.571428571428571,1.),(-0.00308447593286339,0.124708996845866),
 .UNSPECIFIED.);
#162=B_SPLINE_SURFACE_WITH_KNOTS('',3,3,((#14251,#14252,#14253,#14254),
(#14255,#14256,#14257,#14258),(#14259,#14260,#14261,#14262),(#14263,#14264,
#14265,#14266)),.UNSPECIFIED.,.F.,.F.,.F.,(4,4),(4,4),(0.0116899650356219,
0.986620910196183),(0.,0.621418053543664),.UNSPECIFIED.);
#163=B_SPLINE_SURFACE_WITH_KNOTS('',3,3,((#14276,#14277,#14278,#14279),
(#14280,#14281,#14282,#14283),(#14284,#14285,#14286,#14287),(#14288,#14289,
#14290,#14291),(#14292,#14293,#14294,#14295),(#14296,#14297,#14298,#14299)),
 .UNSPECIFIED.,.F.,.F.,.F.,(4,1,1,4),(4,4),(0.,0.285714285714286,0.571428571428571,
1.),(-0.00421817271916687,0.124025126494243),.UNSPECIFIED.);
#164=B_SPLINE_SURFACE_WITH_KNOTS('',3,3,((#14347,#14348,#14349,#14350),
(#14351,#14352,#14353,#14354),(#14355,#14356,#14357,#14358),(#14359,#14360,
#14361,#14362),(#14363,#14364,#14365,#14366)),.UNSPECIFIED.,.F.,.F.,.F.,
(4,1,4),(4,4),(0.,0.571428571428571,1.),(-0.00306862226109154,0.124708996851356),
 .UNSPECIFIED.);
#165=B_SPLINE_SURFACE_WITH_KNOTS('',3,3,((#14400,#14401,#14402,#14403),
(#14404,#14405,#14406,#14407),(#14408,#14409,#14410,#14411),(#14412,#14413,
#14414,#14415),(#14416,#14417,#14418,#14419),(#14420,#14421,#14422,#14423)),
 .UNSPECIFIED.,.F.,.F.,.F.,(4,1,1,4),(4,4),(0.,0.285714285714286,0.571428571428571,
1.),(-0.00430078538920315,0.12402512649425),.UNSPECIFIED.);
#166=B_SPLINE_SURFACE_WITH_KNOTS('',3,3,((#14468,#14469,#14470,#14471),
(#14472,#14473,#14474,#14475),(#14476,#14477,#14478,#14479),(#14480,#14481,
#14482,#14483)),.UNSPECIFIED.,.F.,.F.,.F.,(4,4),(4,4),(0.0133790898038168,
0.988310034964378),(0.,0.621418053491537),.UNSPECIFIED.);
#167=B_SPLINE_SURFACE_WITH_KNOTS('',3,3,((#16866,#16867,#16868,#16869,#16870,
#16871,#16872,#16873,#16874,#16875,#16876,#16877,#16878,#16879,#16880,#16881,
#16882,#16883,#16884,#16885,#16886,#16887,#16888,#16889,#16890,#16891,#16892,
#16893,#16894,#16895,#16896,#16897,#16898,#16899,#16900,#16901,#16902,#16903,
#16904,#16905,#16906,#16907,#16908,#16909,#16910,#16911,#16912,#16913,#16914,
#16915,#16916,#16917,#16918,#16919,#16920,#16921,#16922,#16923,#16924,#16925,
#16926,#16927,#16928,#16929,#16930,#16931,#16932,#16933,#16934,#16935,#16936,
#16937,#16938,#16939,#16940,#16941,#16942,#16943,#16944,#16945,#16946,#16947,
#16948,#16949,#16950,#16951,#16952,#16953,#16954,#16955,#16956,#16957,#16958,
#16959,#16960,#16961,#16962,#16963,#16964,#16965,#16966,#16967,#16968,#16969,
#16970,#16971,#16972,#16973,#16974,#16975,#16976,#16977,#16978,#16979,#16980,
#16981,#16982,#16983,#16984,#16985,#16986,#16987,#16988,#16989,#16990,#16991,
#16992,#16993,#16994,#16995,#16996,#16997,#16998,#16999,#17000,#17001,#17002,
#17003,#17004,#17005,#17006,#17007,#17008,#17009,#17010,#17011,#17012,#17013,
#17014,#17015,#17016,#17017,#17018,#17019,#17020,#17021,#17022,#17023,#17024,
#17025,#17026,#17027,#17028,#17029,#17030,#17031,#17032,#17033,#17034,#17035,
#17036,#17037,#17038,#17039,#17040,#17041,#17042,#17043,#17044,#17045,#17046,
#17047,#17048,#17049,#17050,#17051,#17052,#17053,#17054,#17055,#17056,#17057,
#17058,#17059,#17060,#17061),(#17062,#17063,#17064,#17065,#17066,#17067,
#17068,#17069,#17070,#17071,#17072,#17073,#17074,#17075,#17076,#17077,#17078,
#17079,#17080,#17081,#17082,#17083,#17084,#17085,#17086,#17087,#17088,#17089,
#17090,#17091,#17092,#17093,#17094,#17095,#17096,#17097,#17098,#17099,#17100,
#17101,#17102,#17103,#17104,#17105,#17106,#17107,#17108,#17109,#17110,#17111,
#17112,#17113,#17114,#17115,#17116,#17117,#17118,#17119,#17120,#17121,#17122,
#17123,#17124,#17125,#17126,#17127,#17128,#17129,#17130,#17131,#17132,#17133,
#17134,#17135,#17136,#17137,#17138,#17139,#17140,#17141,#17142,#17143,#17144,
#17145,#17146,#17147,#17148,#17149,#17150,#17151,#17152,#17153,#17154,#17155,
#17156,#17157,#17158,#17159,#17160,#17161,#17162,#17163,#17164,#17165,#17166,
#17167,#17168,#17169,#17170,#17171,#17172,#17173,#17174,#17175,#17176,#17177,
#17178,#17179,#17180,#17181,#17182,#17183,#17184,#17185,#17186,#17187,#17188,
#17189,#17190,#17191,#17192,#17193,#17194,#17195,#17196,#17197,#17198,#17199,
#17200,#17201,#17202,#17203,#17204,#17205,#17206,#17207,#17208,#17209,#17210,
#17211,#17212,#17213,#17214,#17215,#17216,#17217,#17218,#17219,#17220,#17221,
#17222,#17223,#17224,#17225,#17226,#17227,#17228,#17229,#17230,#17231,#17232,
#17233,#17234,#17235,#17236,#17237,#17238,#17239,#17240,#17241,#17242,#17243,
#17244,#17245,#17246,#17247,#17248,#17249,#17250,#17251,#17252,#17253,#17254,
#17255,#17256,#17257),(#17258,#17259,#17260,#17261,#17262,#17263,#17264,
#17265,#17266,#17267,#17268,#17269,#17270,#17271,#17272,#17273,#17274,#17275,
#17276,#17277,#17278,#17279,#17280,#17281,#17282,#17283,#17284,#17285,#17286,
#17287,#17288,#17289,#17290,#17291,#17292,#17293,#17294,#17295,#17296,#17297,
#17298,#17299,#17300,#17301,#17302,#17303,#17304,#17305,#17306,#17307,#17308,
#17309,#17310,#17311,#17312,#17313,#17314,#17315,#17316,#17317,#17318,#17319,
#17320,#17321,#17322,#17323,#17324,#17325,#17326,#17327,#17328,#17329,#17330,
#17331,#17332,#17333,#17334,#17335,#17336,#17337,#17338,#17339,#17340,#17341,
#17342,#17343,#17344,#17345,#17346,#17347,#17348,#17349,#17350,#17351,#17352,
#17353,#17354,#17355,#17356,#17357,#17358,#17359,#17360,#17361,#17362,#17363,
#17364,#17365,#17366,#17367,#17368,#17369,#17370,#17371,#17372,#17373,#17374,
#17375,#17376,#17377,#17378,#17379,#17380,#17381,#17382,#17383,#17384,#17385,
#17386,#17387,#17388,#17389,#17390,#17391,#17392,#17393,#17394,#17395,#17396,
#17397,#17398,#17399,#17400,#17401,#17402,#17403,#17404,#17405,#17406,#17407,
#17408,#17409,#17410,#17411,#17412,#17413,#17414,#17415,#17416,#17417,#17418,
#17419,#17420,#17421,#17422,#17423,#17424,#17425,#17426,#17427,#17428,#17429,
#17430,#17431,#17432,#17433,#17434,#17435,#17436,#17437,#17438,#17439,#17440,
#17441,#17442,#17443,#17444,#17445,#17446,#17447,#17448,#17449,#17450,#17451,
#17452,#17453),(#17454,#17455,#17456,#17457,#17458,#17459,#17460,#17461,
#17462,#17463,#17464,#17465,#17466,#17467,#17468,#17469,#17470,#17471,#17472,
#17473,#17474,#17475,#17476,#17477,#17478,#17479,#17480,#17481,#17482,#17483,
#17484,#17485,#17486,#17487,#17488,#17489,#17490,#17491,#17492,#17493,#17494,
#17495,#17496,#17497,#17498,#17499,#17500,#17501,#17502,#17503,#17504,#17505,
#17506,#17507,#17508,#17509,#17510,#17511,#17512,#17513,#17514,#17515,#17516,
#17517,#17518,#17519,#17520,#17521,#17522,#17523,#17524,#17525,#17526,#17527,
#17528,#17529,#17530,#17531,#17532,#17533,#17534,#17535,#17536,#17537,#17538,
#17539,#17540,#17541,#17542,#17543,#17544,#17545,#17546,#17547,#17548,#17549,
#17550,#17551,#17552,#17553,#17554,#17555,#17556,#17557,#17558,#17559,#17560,
#17561,#17562,#17563,#17564,#17565,#17566,#17567,#17568,#17569,#17570,#17571,
#17572,#17573,#17574,#17575,#17576,#17577,#17578,#17579,#17580,#17581,#17582,
#17583,#17584,#17585,#17586,#17587,#17588,#17589,#17590,#17591,#17592,#17593,
#17594,#17595,#17596,#17597,#17598,#17599,#17600,#17601,#17602,#17603,#17604,
#17605,#17606,#17607,#17608,#17609,#17610,#17611,#17612,#17613,#17614,#17615,
#17616,#17617,#17618,#17619,#17620,#17621,#17622,#17623,#17624,#17625,#17626,
#17627,#17628,#17629,#17630,#17631,#17632,#17633,#17634,#17635,#17636,#17637,
#17638,#17639,#17640,#17641,#17642,#17643,#17644,#17645,#17646,#17647,#17648,
#17649)),.UNSPECIFIED.,.F.,.F.,.F.,(4,4),(4,1,1,1,1,1,1,1,1,1,1,1,1,1,1,
1,1,1,1,1,1,1,1,1,1,1,1,1,1,1,1,1,1,1,1,1,1,1,1,1,1,1,1,1,1,1,1,1,1,1,1,
1,1,1,1,1,1,1,1,1,1,1,1,1,1,1,1,1,1,1,1,1,1,1,1,1,1,1,1,1,1,1,1,1,1,1,1,
1,1,1,1,1,1,1,1,1,1,1,1,1,1,1,1,1,1,1,1,1,1,1,1,1,1,1,1,1,1,1,1,1,1,1,1,
1,1,1,1,1,1,1,1,1,1,1,1,1,1,1,1,1,1,1,1,1,1,1,1,1,1,1,1,1,1,1,1,1,1,1,1,
1,1,1,1,1,1,1,1,1,1,1,1,1,1,1,1,1,1,1,1,1,1,1,1,1,1,1,1,1,1,1,1,1,1,4),
(0.,0.0329955678841871),(11.6159397475006,12.61358260836,13.6112254692194,
14.6088683300789,15.6065111909383,16.6041540517977,17.6017969126571,18.5994397735165,
19.5970826343759,20.5947254952353,21.5923683560947,22.5900112169541,23.5876540778135,
24.5852969386729,25.5829397995323,26.5805826603917,27.5782255212511,28.5758683821105,
29.5735112429699,30.5711541038294,31.5687969646888,32.5664398255482,33.5640826864076,
34.561725547267,35.5593684081264,36.5570112689858,37.5546541298452,38.5522969907046,
39.549939851564,40.5475827124234,41.5452255732828,42.5428684341422,43.5405112950016,
44.538154155861,45.5357970167204,46.5334398775799,47.5310827384393,48.5287255992987,
49.5263684601581,50.5240113210175,51.5216541818769,52.5192970427363,53.5169399035957,
54.5145827644551,55.5122256253145,56.5098684861739,57.5075113470333,58.5051542078927,
59.5027970687521,60.5004399296115,61.4980827904709,62.4957256513303,63.4933685121897,
64.4910113730492,65.4886542339086,66.486297094768,67.4839399556274,68.4815828164868,
69.4792256773462,70.4768685382056,71.474511399065,72.4721542599244,73.4697971207838,
74.4674399816432,75.4650828425026,76.462725703362,77.4603685642214,78.4580114250808,
79.4556542859402,80.4532971467996,81.4509400076591,82.4485828685185,83.4462257293779,
84.4438685902373,85.4415114510967,86.4391543119561,87.4367971728155,88.4344400336749,
89.4320828945343,90.4297257553937,91.4273686162531,92.4250114771125,93.4226543379719,
94.4202971988313,95.4179400596907,96.4155829205502,97.4132257814096,98.410868642269,
99.4085115031284,100.406154363988,101.403797224847,102.401440085707,103.399082946566,
104.396725807425,105.394368668285,106.392011529144,107.389654390004,108.387297250863,
109.384940111722,110.382582972582,111.380225833441,112.377868694301,113.37551155516,
114.373154416019,115.370797276879,116.368440137738,117.366082998598,118.363725859457,
119.361368720316,120.359011581176,121.356654442035,122.354297302895,123.351940163754,
124.349583024614,125.347225885473,126.344868746332,127.342511607192,128.340154468051,
129.337797328911,130.33544018977,131.333083050629,132.330725911489,133.328368772348,
134.326011633208,135.323654494067,136.321297354926,137.318940215786,138.316583076645,
139.314225937505,140.311868798364,141.309511659223,142.307154520083,143.304797380942,
144.302440241802,145.300083102661,146.29772596352,147.29536882438,148.293011685239,
149.290654546099,150.288297406958,151.285940267817,152.283583128677,153.281225989536,
154.278868850396,155.276511711255,156.274154572115,157.271797432974,158.269440293833,
159.267083154693,160.264726015552,161.262368876412,162.260011737271,163.25765459813,
164.25529745899,165.252940319849,166.250583180709,167.248226041568,168.245868902427,
169.243511763287,170.241154624146,171.238797485006,172.236440345865,173.234083206724,
174.231726067584,175.229368928443,176.227011789303,177.224654650162,178.222297511021,
179.219940371881,180.21758323274,181.2152260936,182.212868954459,183.210511815318,
184.208154676178,185.205797537037,186.203440397897,187.201083258756,188.198726119616,
189.196368980475,190.194011841334,191.191654702194,192.189297563053,193.186940423913,
194.184583284772,195.182226145631,196.179869006491,197.17751186735,198.17515472821,
199.172797589069,200.170440449928,201.168083310788,202.165726171647,203.163369032507,
204.161011893366),.UNSPECIFIED.);
#168=B_SPLINE_SURFACE_WITH_KNOTS('',3,3,((#17739,#17740,#17741,#17742,#17743,
#17744,#17745,#17746,#17747,#17748,#17749,#17750,#17751,#17752,#17753,#17754,
#17755,#17756,#17757,#17758,#17759,#17760,#17761,#17762,#17763,#17764,#17765,
#17766,#17767,#17768,#17769,#17770,#17771,#17772,#17773,#17774,#17775,#17776,
#17777,#17778,#17779,#17780,#17781,#17782,#17783,#17784,#17785,#17786,#17787,
#17788,#17789,#17790,#17791,#17792,#17793,#17794,#17795,#17796,#17797,#17798,
#17799,#17800,#17801,#17802,#17803,#17804,#17805,#17806,#17807,#17808,#17809,
#17810,#17811,#17812,#17813,#17814,#17815,#17816,#17817,#17818,#17819,#17820,
#17821,#17822,#17823,#17824,#17825,#17826,#17827,#17828,#17829,#17830,#17831,
#17832,#17833,#17834,#17835,#17836,#17837,#17838,#17839,#17840,#17841,#17842,
#17843,#17844,#17845,#17846,#17847,#17848,#17849,#17850,#17851,#17852,#17853,
#17854,#17855,#17856,#17857,#17858,#17859,#17860,#17861,#17862,#17863,#17864,
#17865,#17866,#17867,#17868,#17869,#17870,#17871,#17872,#17873,#17874,#17875,
#17876,#17877,#17878,#17879,#17880,#17881,#17882,#17883,#17884,#17885,#17886,
#17887,#17888,#17889,#17890,#17891,#17892,#17893,#17894,#17895,#17896,#17897,
#17898,#17899,#17900,#17901,#17902,#17903,#17904,#17905,#17906,#17907,#17908,
#17909,#17910,#17911,#17912,#17913,#17914,#17915,#17916,#17917,#17918,#17919,
#17920,#17921,#17922,#17923,#17924,#17925,#17926,#17927,#17928,#17929,#17930,
#17931,#17932,#17933,#17934,#17935,#17936),(#17937,#17938,#17939,#17940,
#17941,#17942,#17943,#17944,#17945,#17946,#17947,#17948,#17949,#17950,#17951,
#17952,#17953,#17954,#17955,#17956,#17957,#17958,#17959,#17960,#17961,#17962,
#17963,#17964,#17965,#17966,#17967,#17968,#17969,#17970,#17971,#17972,#17973,
#17974,#17975,#17976,#17977,#17978,#17979,#17980,#17981,#17982,#17983,#17984,
#17985,#17986,#17987,#17988,#17989,#17990,#17991,#17992,#17993,#17994,#17995,
#17996,#17997,#17998,#17999,#18000,#18001,#18002,#18003,#18004,#18005,#18006,
#18007,#18008,#18009,#18010,#18011,#18012,#18013,#18014,#18015,#18016,#18017,
#18018,#18019,#18020,#18021,#18022,#18023,#18024,#18025,#18026,#18027,#18028,
#18029,#18030,#18031,#18032,#18033,#18034,#18035,#18036,#18037,#18038,#18039,
#18040,#18041,#18042,#18043,#18044,#18045,#18046,#18047,#18048,#18049,#18050,
#18051,#18052,#18053,#18054,#18055,#18056,#18057,#18058,#18059,#18060,#18061,
#18062,#18063,#18064,#18065,#18066,#18067,#18068,#18069,#18070,#18071,#18072,
#18073,#18074,#18075,#18076,#18077,#18078,#18079,#18080,#18081,#18082,#18083,
#18084,#18085,#18086,#18087,#18088,#18089,#18090,#18091,#18092,#18093,#18094,
#18095,#18096,#18097,#18098,#18099,#18100,#18101,#18102,#18103,#18104,#18105,
#18106,#18107,#18108,#18109,#18110,#18111,#18112,#18113,#18114,#18115,#18116,
#18117,#18118,#18119,#18120,#18121,#18122,#18123,#18124,#18125,#18126,#18127,
#18128,#18129,#18130,#18131,#18132,#18133,#18134),(#18135,#18136,#18137,
#18138,#18139,#18140,#18141,#18142,#18143,#18144,#18145,#18146,#18147,#18148,
#18149,#18150,#18151,#18152,#18153,#18154,#18155,#18156,#18157,#18158,#18159,
#18160,#18161,#18162,#18163,#18164,#18165,#18166,#18167,#18168,#18169,#18170,
#18171,#18172,#18173,#18174,#18175,#18176,#18177,#18178,#18179,#18180,#18181,
#18182,#18183,#18184,#18185,#18186,#18187,#18188,#18189,#18190,#18191,#18192,
#18193,#18194,#18195,#18196,#18197,#18198,#18199,#18200,#18201,#18202,#18203,
#18204,#18205,#18206,#18207,#18208,#18209,#18210,#18211,#18212,#18213,#18214,
#18215,#18216,#18217,#18218,#18219,#18220,#18221,#18222,#18223,#18224,#18225,
#18226,#18227,#18228,#18229,#18230,#18231,#18232,#18233,#18234,#18235,#18236,
#18237,#18238,#18239,#18240,#18241,#18242,#18243,#18244,#18245,#18246,#18247,
#18248,#18249,#18250,#18251,#18252,#18253,#18254,#18255,#18256,#18257,#18258,
#18259,#18260,#18261,#18262,#18263,#18264,#18265,#18266,#18267,#18268,#18269,
#18270,#18271,#18272,#18273,#18274,#18275,#18276,#18277,#18278,#18279,#18280,
#18281,#18282,#18283,#18284,#18285,#18286,#18287,#18288,#18289,#18290,#18291,
#18292,#18293,#18294,#18295,#18296,#18297,#18298,#18299,#18300,#18301,#18302,
#18303,#18304,#18305,#18306,#18307,#18308,#18309,#18310,#18311,#18312,#18313,
#18314,#18315,#18316,#18317,#18318,#18319,#18320,#18321,#18322,#18323,#18324,
#18325,#18326,#18327,#18328,#18329,#18330,#18331,#18332),(#18333,#18334,
#18335,#18336,#18337,#18338,#18339,#18340,#18341,#18342,#18343,#18344,#18345,
#18346,#18347,#18348,#18349,#18350,#18351,#18352,#18353,#18354,#18355,#18356,
#18357,#18358,#18359,#18360,#18361,#18362,#18363,#18364,#18365,#18366,#18367,
#18368,#18369,#18370,#18371,#18372,#18373,#18374,#18375,#18376,#18377,#18378,
#18379,#18380,#18381,#18382,#18383,#18384,#18385,#18386,#18387,#18388,#18389,
#18390,#18391,#18392,#18393,#18394,#18395,#18396,#18397,#18398,#18399,#18400,
#18401,#18402,#18403,#18404,#18405,#18406,#18407,#18408,#18409,#18410,#18411,
#18412,#18413,#18414,#18415,#18416,#18417,#18418,#18419,#18420,#18421,#18422,
#18423,#18424,#18425,#18426,#18427,#18428,#18429,#18430,#18431,#18432,#18433,
#18434,#18435,#18436,#18437,#18438,#18439,#18440,#18441,#18442,#18443,#18444,
#18445,#18446,#18447,#18448,#18449,#18450,#18451,#18452,#18453,#18454,#18455,
#18456,#18457,#18458,#18459,#18460,#18461,#18462,#18463,#18464,#18465,#18466,
#18467,#18468,#18469,#18470,#18471,#18472,#18473,#18474,#18475,#18476,#18477,
#18478,#18479,#18480,#18481,#18482,#18483,#18484,#18485,#18486,#18487,#18488,
#18489,#18490,#18491,#18492,#18493,#18494,#18495,#18496,#18497,#18498,#18499,
#18500,#18501,#18502,#18503,#18504,#18505,#18506,#18507,#18508,#18509,#18510,
#18511,#18512,#18513,#18514,#18515,#18516,#18517,#18518,#18519,#18520,#18521,
#18522,#18523,#18524,#18525,#18526,#18527,#18528,#18529,#18530)),
 .UNSPECIFIED.,.F.,.F.,.F.,(4,4),(4,1,1,1,1,1,1,1,1,1,1,1,1,1,1,1,1,1,1,
1,1,1,1,1,1,1,1,1,1,1,1,1,1,1,1,1,1,1,1,1,1,1,1,1,1,1,1,1,1,1,1,1,1,1,1,
1,1,1,1,1,1,1,1,1,1,1,1,1,1,1,1,1,1,1,1,1,1,1,1,1,1,1,1,1,1,1,1,1,1,1,1,
1,1,1,1,1,1,1,1,1,1,1,1,1,1,1,1,1,1,1,1,1,1,1,1,1,1,1,1,1,1,1,1,1,1,1,1,
1,1,1,1,1,1,1,1,1,1,1,1,1,1,1,1,1,1,1,1,1,1,1,1,1,1,1,1,1,1,1,1,1,1,1,1,
1,1,1,1,1,1,1,1,1,1,1,1,1,1,1,1,1,1,1,1,1,1,1,1,1,1,1,1,1,1,1,1,4),(0.,
0.0329955678841871),(8.30203615430855,9.30007843543257,10.2981207165566,
11.2961629976806,12.2942052788047,13.2922475599287,14.2902898410527,15.2883321221767,
16.2863744033008,17.2844166844248,18.2824589655488,19.2805012466728,20.2785435277969,
21.2765858089209,22.2746280900449,23.272670371169,24.270712652293,25.268754933417,
26.266797214541,27.2648394956651,28.2628817767891,29.2609240579131,30.2589663390371,
31.2570086201612,32.2550509012852,33.2530931824092,34.2511354635333,35.2491777446573,
36.2472200257813,37.2452623069053,38.2433045880294,39.2413468691534,40.2393891502774,
41.2374314314014,42.2354737125255,43.2335159936495,44.2315582747735,45.2296005558975,
46.2276428370216,47.2256851181456,48.2237273992696,49.2217696803937,50.2198119615177,
51.2178542426417,52.2158965237657,53.2139388048898,54.2119810860138,55.2100233671378,
56.2080656482619,57.2061079293859,58.2041502105099,59.2021924916339,60.200234772758,
61.198277053882,62.196319335006,63.19436161613,64.1924038972541,65.1904461783781,
66.1884884595021,67.1865307406262,68.1845730217502,69.1826153028742,70.1806575839982,
71.1786998651223,72.1767421462463,73.1747844273703,74.1728267084943,75.1708689896184,
76.1689112707424,77.1669535518664,78.1649958329905,79.1630381141145,80.1610803952385,
81.1591226763625,82.1571649574865,83.1552072386106,84.1532495197346,85.1512918008586,
86.1493340819827,87.1473763631067,88.1454186442307,89.1434609253548,90.1415032064788,
91.1395454876028,92.1375877687268,93.1356300498508,94.1336723309749,95.1317146120989,
96.1297568932229,97.127799174347,98.125841455471,99.123883736595,100.121926017719,
101.119968298843,102.118010579967,103.116052861091,104.114095142215,105.112137423339,
106.110179704463,107.108221985587,108.106264266711,109.104306547835,110.102348828959,
111.100391110083,112.098433391207,113.096475672331,114.094517953455,115.092560234579,
116.090602515703,117.088644796828,118.086687077952,119.084729359076,120.0827716402,
121.080813921324,122.078856202448,123.076898483572,124.074940764696,125.07298304582,
126.071025326944,127.069067608068,128.067109889192,129.065152170316,130.06319445144,
131.061236732564,132.059279013688,133.057321294812,134.055363575936,135.05340585706,
136.051448138184,137.049490419308,138.047532700432,139.045574981556,140.04361726268,
141.041659543804,142.039701824928,143.037744106052,144.035786387176,145.0338286683,
146.031870949424,147.029913230548,148.027955511672,149.025997792796,150.02404007392,
151.022082355044,152.020124636168,153.018166917292,154.016209198417,155.014251479541,
156.012293760665,157.010336041789,158.008378322913,159.006420604037,160.004462885161,
161.002505166285,162.000547447409,162.998589728533,163.996632009657,164.994674290781,
165.992716571905,166.990758853029,167.988801134153,168.986843415277,169.984885696401,
170.982927977525,171.980970258649,172.979012539773,173.977054820897,174.975097102021,
175.973139383145,176.971181664269,177.969223945393,178.967266226517,179.965308507641,
180.963350788765,181.961393069889,182.959435351013,183.957477632137,184.955519913261,
185.953562194385,186.951604475509,187.949646756633,188.947689037757,189.945731318881,
190.943773600006,191.94181588113,192.939858162254,193.937900443378,194.935942724502,
195.933985005626,196.93202728675,197.930069567874,198.928111848998,199.926154130122,
200.924196411246,201.92223869237,202.920280973494),.UNSPECIFIED.);
#169=B_SPLINE_SURFACE_WITH_KNOTS('',3,3,((#18989,#18990,#18991,#18992,#18993,
#18994,#18995,#18996,#18997,#18998,#18999,#19000,#19001,#19002,#19003,#19004,
#19005,#19006,#19007,#19008,#19009,#19010,#19011,#19012,#19013,#19014,#19015,
#19016,#19017,#19018,#19019,#19020,#19021,#19022,#19023,#19024),(#19025,
#19026,#19027,#19028,#19029,#19030,#19031,#19032,#19033,#19034,#19035,#19036,
#19037,#19038,#19039,#19040,#19041,#19042,#19043,#19044,#19045,#19046,#19047,
#19048,#19049,#19050,#19051,#19052,#19053,#19054,#19055,#19056,#19057,#19058,
#19059,#19060),(#19061,#19062,#19063,#19064,#19065,#19066,#19067,#19068,
#19069,#19070,#19071,#19072,#19073,#19074,#19075,#19076,#19077,#19078,#19079,
#19080,#19081,#19082,#19083,#19084,#19085,#19086,#19087,#19088,#19089,#19090,
#19091,#19092,#19093,#19094,#19095,#19096),(#19097,#19098,#19099,#19100,
#19101,#19102,#19103,#19104,#19105,#19106,#19107,#19108,#19109,#19110,#19111,
#19112,#19113,#19114,#19115,#19116,#19117,#19118,#19119,#19120,#19121,#19122,
#19123,#19124,#19125,#19126,#19127,#19128,#19129,#19130,#19131,#19132)),
 .UNSPECIFIED.,.F.,.F.,.F.,(4,4),(4,1,1,1,1,1,1,1,1,1,1,1,1,1,1,1,1,1,1,
1,1,1,1,1,1,1,1,1,1,1,1,1,1,4),(0.,0.0321584099938622),(11.8553612635794,
12.830508595889,13.8056559281987,14.7808032605084,15.755950592818,16.7310979251277,
17.7062452574374,18.681392589747,19.6565399220567,20.6316872543664,21.606834586676,
22.5819819189857,23.5571292512954,24.532276583605,25.5074239159147,26.4825712482243,
27.457718580534,28.4328659128437,29.4080132451533,30.383160577463,31.3583079097727,
32.3334552420823,33.308602574392,34.2837499067017,35.2588972390113,36.234044571321,
37.2091919036307,38.1843392359403,39.15948656825,40.1346339005596,41.1097812328693,
42.084928565179,43.0600758974886,44.0352232297983),.UNSPECIFIED.);
#170=B_SPLINE_SURFACE_WITH_KNOTS('',3,3,((#19256,#19257,#19258,#19259,#19260,
#19261,#19262,#19263,#19264,#19265,#19266,#19267,#19268,#19269,#19270,#19271,
#19272,#19273,#19274,#19275,#19276,#19277,#19278,#19279,#19280,#19281,#19282,
#19283,#19284,#19285,#19286,#19287,#19288,#19289,#19290,#19291),(#19292,
#19293,#19294,#19295,#19296,#19297,#19298,#19299,#19300,#19301,#19302,#19303,
#19304,#19305,#19306,#19307,#19308,#19309,#19310,#19311,#19312,#19313,#19314,
#19315,#19316,#19317,#19318,#19319,#19320,#19321,#19322,#19323,#19324,#19325,
#19326,#19327),(#19328,#19329,#19330,#19331,#19332,#19333,#19334,#19335,
#19336,#19337,#19338,#19339,#19340,#19341,#19342,#19343,#19344,#19345,#19346,
#19347,#19348,#19349,#19350,#19351,#19352,#19353,#19354,#19355,#19356,#19357,
#19358,#19359,#19360,#19361,#19362,#19363),(#19364,#19365,#19366,#19367,
#19368,#19369,#19370,#19371,#19372,#19373,#19374,#19375,#19376,#19377,#19378,
#19379,#19380,#19381,#19382,#19383,#19384,#19385,#19386,#19387,#19388,#19389,
#19390,#19391,#19392,#19393,#19394,#19395,#19396,#19397,#19398,#19399)),
 .UNSPECIFIED.,.F.,.F.,.F.,(4,4),(4,1,1,1,1,1,1,1,1,1,1,1,1,1,1,1,1,1,1,
1,1,1,1,1,1,1,1,1,1,1,1,1,1,4),(0.,0.0321584099938622),(14.3984001269719,
15.3735474592815,16.3486947915912,17.3238421239009,18.2989894562105,19.2741367885202,
20.2492841208299,21.2244314531395,22.1995787854492,23.1747261177589,24.1498734500685,
25.1250207823782,26.1001681146879,27.0753154469975,28.0504627793072,29.0256101116168,
30.0007574439265,30.9759047762362,31.9510521085458,32.9261994408555,33.9013467731652,
34.8764941054748,35.8516414377845,36.8267887700942,37.8019361024038,38.7770834347135,
39.7522307670232,40.7273780993328,41.7025254316425,42.6776727639522,43.6528200962618,
44.6279674285715,45.6031147608811,46.5782620931908),.UNSPECIFIED.);
#171=B_SPLINE_CURVE_WITH_KNOTS('',3,(#9725,#9726,#9727,#9728),
 .UNSPECIFIED.,.F.,.F.,(4,4),(3.28016616408593,4.26236080300681),
 .UNSPECIFIED.);
#172=B_SPLINE_CURVE_WITH_KNOTS('',3,(#9732,#9733,#9734,#9735),
 .UNSPECIFIED.,.F.,.F.,(4,4),(8.92392608805945,9.90612072688831),
 .UNSPECIFIED.);
#173=B_SPLINE_CURVE_WITH_KNOTS('',3,(#9737,#9738,#9739,#9740,#9741,#9742,
#9743,#9744,#9745,#9746,#9747,#9748,#9749,#9750,#9751,#9752,#9753,#9754,
#9755),.UNSPECIFIED.,.F.,.F.,(4,3,3,3,3,3,4),(-0.050768112872884,-0.0388528786649772,
-0.0311058171716578,-0.0259830388669653,-0.0210744122964195,-0.0143837148934404,
0.),.UNSPECIFIED.);
#174=B_SPLINE_CURVE_WITH_KNOTS('',3,(#9757,#9758,#9759,#9760),
 .UNSPECIFIED.,.F.,.F.,(4,4),(9.9568018127159,12.1251256661408),
 .UNSPECIFIED.);
#175=B_SPLINE_CURVE_WITH_KNOTS('',3,(#9764,#9765,#9766,#9767),
 .UNSPECIFIED.,.F.,.F.,(4,4),(1.06116122492545,3.22948508825557),
 .UNSPECIFIED.);
#176=B_SPLINE_CURVE_WITH_KNOTS('',3,(#9768,#9769,#9770,#9771,#9772,#9773,
#9774,#9775,#9776,#9777,#9778,#9779,#9780,#9781,#9782,#9783,#9784,#9785,
#9786),.UNSPECIFIED.,.F.,.F.,(4,3,3,3,3,3,4),(-0.0507681129736439,-0.0388528772897764,
-0.0311058147321604,-0.0259830361493327,-0.0210744097201194,-0.0143837130754026,
-9.90506278315E-9),.UNSPECIFIED.);
#177=B_SPLINE_CURVE_WITH_KNOTS('',3,(#9934,#9935,#9936,#9937,#9938,#9939),
 .UNSPECIFIED.,.F.,.F.,(4,2,4),(-0.605566356596631,-0.303329629920269,-0.000148729590407126),
 .UNSPECIFIED.);
#178=B_SPLINE_CURVE_WITH_KNOTS('',3,(#9941,#9942,#9943,#9944,#9945,#9946,
#9947,#9948,#9949,#9950,#9951,#9952,#9953,#9954,#9955,#9956,#9957,#9958,
#9959,#9960,#9961,#9962,#9963,#9964,#9965,#9966,#9967,#9968),
 .UNSPECIFIED.,.F.,.F.,(4,3,3,3,3,3,3,3,3,4),(-0.153210533292091,-0.129383071834804,
-0.117098895005168,-0.0931297672424715,-0.0778761857300216,-0.065564095006876,
-0.0417435583396367,-0.038874550231651,-0.0150983388519663,0.),
 .UNSPECIFIED.);
#179=B_SPLINE_CURVE_WITH_KNOTS('',3,(#9972,#9973,#9974,#9975,#9976,#9977,
#9978,#9979,#9980,#9981,#9982,#9983,#9984,#9985,#9986,#9987,#9988,#9989,
#9990,#9991,#9992,#9993,#9994,#9995,#9996,#9997,#9998,#9999),
 .UNSPECIFIED.,.F.,.F.,(4,3,3,3,3,3,3,3,3,4),(-0.153244081227051,-0.129493605146206,
-0.117970006482883,-0.0941492904140308,-0.0876825809854227,-0.078828741443105,
-0.0548877675055393,-0.0394694906046094,-0.0155984926894347,0.),
 .UNSPECIFIED.);
#180=B_SPLINE_CURVE_WITH_KNOTS('',3,(#10000,#10001,#10002,#10003,#10004,
#10005),.UNSPECIFIED.,.F.,.F.,(4,2,4),(-0.606539490527658,-0.303329031627741,
-0.00112184825655631),.UNSPECIFIED.);
#181=B_SPLINE_CURVE_WITH_KNOTS('',3,(#10010,#10011,#10012,#10013,#10014,
#10015),.UNSPECIFIED.,.F.,.F.,(4,2,4),(-0.606785247764818,-0.303663188081886,
-0.00088649083675002),.UNSPECIFIED.);
#182=B_SPLINE_CURVE_WITH_KNOTS('',3,(#10017,#10018,#10019,#10020,#10021,
#10022,#10023,#10024,#10025,#10026,#10027,#10028,#10029,#10030,#10031,#10032,
#10033,#10034,#10035,#10036,#10037,#10038,#10039,#10040,#10041,#10042,#10043,
#10044),.UNSPECIFIED.,.F.,.F.,(4,3,3,3,3,3,3,3,3,4),(-0.15258577077829,
-0.128839317352572,-0.117158786685373,-0.0932148261566644,-0.0780319390000633,
-0.0653676349965338,-0.0415665498371782,-0.0389909618069961,-0.0152059030050533,
0.),.UNSPECIFIED.);
#183=B_SPLINE_CURVE_WITH_KNOTS('',3,(#10048,#10049,#10050,#10051,#10052,
#10053,#10054,#10055,#10056,#10057,#10058,#10059,#10060,#10061,#10062,#10063,
#10064,#10065,#10066,#10067,#10068,#10069,#10070,#10071,#10072,#10073,#10074,
#10075),.UNSPECIFIED.,.F.,.F.,(4,3,3,3,3,3,3,3,3,4),(-0.152596853546747,
-0.128825864440686,-0.115507515430042,-0.0917263797372463,-0.0872428123353572,
-0.0783995504057471,-0.0544835945915644,-0.0392209901554083,-0.0154275313391792,
0.),.UNSPECIFIED.);
#184=B_SPLINE_CURVE_WITH_KNOTS('',3,(#10077,#10078,#10079,#10080,#10081,
#10082),.UNSPECIFIED.,.F.,.F.,(4,2,4),(-0.606440835737524,-0.303663090452391,
-0.000542069086802599),.UNSPECIFIED.);
#185=B_SPLINE_CURVE_WITH_KNOTS('',3,(#10088,#10089,#10090,#10091,#10092,
#10093),.UNSPECIFIED.,.F.,.F.,(4,2,4),(-0.607379220946441,-0.303761646676304,
-0.00124422999587004),.UNSPECIFIED.);
#186=B_SPLINE_CURVE_WITH_KNOTS('',3,(#10095,#10096,#10097,#10098,#10099,
#10100,#10101,#10102,#10103,#10104,#10105,#10106,#10107,#10108,#10109,#10110,
#10111,#10112,#10113,#10114,#10115,#10116,#10117,#10118,#10119,#10120,#10121,
#10122),.UNSPECIFIED.,.F.,.F.,(4,3,3,3,3,3,3,3,3,4),(-0.152287640102895,
-0.128554450486317,-0.115193035178751,-0.0912770810520543,-0.0781028969167454,
-0.0652733399726575,-0.0414820896655672,-0.0390446621366508,-0.0152552334863041,
0.),.UNSPECIFIED.);
#187=B_SPLINE_CURVE_WITH_KNOTS('',3,(#10126,#10127,#10128,#10129,#10130,
#10131,#10132,#10133,#10134,#10135,#10136,#10137,#10138,#10139,#10140,#10141,
#10142,#10143,#10144,#10145,#10146,#10147,#10148,#10149,#10150,#10151,#10152,
#10153),.UNSPECIFIED.,.F.,.F.,(4,3,3,3,3,3,3,3,3,4),(-0.152291020205185,
-0.128517753946702,-0.115248901231919,-0.0914807886786037,-0.0870359119466785,
-0.0782017654295232,-0.054298407767766,-0.03910658747416,-0.0153486482327859,
0.),.UNSPECIFIED.);
#188=B_SPLINE_CURVE_WITH_KNOTS('',3,(#10155,#10156,#10157,#10158,#10159,
#10160),.UNSPECIFIED.,.F.,.F.,(4,2,4),(-0.606279550122448,-0.303761677523001,
-0.000144559171857295),.UNSPECIFIED.);
#189=B_SPLINE_CURVE_WITH_KNOTS('',3,(#10166,#10167,#10168,#10169,#10170,
#10171),.UNSPECIFIED.,.F.,.F.,(4,2,4),(-0.607536685592867,-0.303784463250135,
-0.00133982193348342),.UNSPECIFIED.);
#190=B_SPLINE_CURVE_WITH_KNOTS('',3,(#10172,#10173,#10174,#10175,#10176,
#10177,#10178,#10179,#10180,#10181,#10182,#10183,#10184,#10185,#10186,#10187,
#10188,#10189,#10190,#10191,#10192,#10193,#10194,#10195,#10196,#10197,#10198,
#10199),.UNSPECIFIED.,.F.,.F.,(4,3,3,3,3,3,3,3,3,4),(-0.152217684890348,
-0.128490376540845,-0.11516578527262,-0.091253137134092,-0.0781160865160423,
-0.0652495101170982,-0.0414606291875136,-0.0390546905501479,-0.015263466236765,
0.),.UNSPECIFIED.);
#191=B_SPLINE_CURVE_WITH_KNOTS('',3,(#10201,#10202,#10203,#10204,#10205,
#10206,#10207,#10208,#10209,#10210,#10211,#10212,#10213,#10214,#10215,#10216,
#10217,#10218,#10219,#10220,#10221,#10222,#10223,#10224,#10225,#10226,#10227,
#10228),.UNSPECIFIED.,.F.,.F.,(4,3,3,3,3,3,3,3,3,4),(-0.152219351639196,
-0.128444680332832,-0.115193337419806,-0.0914284185691762,-0.0869890032859244,
-0.0781648487722283,-0.0542647883944502,-0.0390852411900305,-0.0153331469286526,
0.),.UNSPECIFIED.);
#192=B_SPLINE_CURVE_WITH_KNOTS('',3,(#10230,#10231,#10232,#10233,#10234,
#10235),.UNSPECIFIED.,.F.,.F.,(4,2,4),(-0.606231877025315,-0.303784501204342,
-3.50089943914611E-5),.UNSPECIFIED.);
#193=B_SPLINE_CURVE_WITH_KNOTS('',3,(#10241,#10242,#10243,#10244),
 .UNSPECIFIED.,.F.,.F.,(4,4),(0.0108333608245492,0.617725317592517),
 .UNSPECIFIED.);
#194=B_SPLINE_CURVE_WITH_KNOTS('',3,(#10248,#10249,#10250,#10251),
 .UNSPECIFIED.,.F.,.F.,(4,4),(-0.617725317592517,-0.0108333608245492),
 .UNSPECIFIED.);
#195=B_SPLINE_CURVE_WITH_KNOTS('',3,(#10254,#10255,#10256,#10257),
 .UNSPECIFIED.,.F.,.F.,(4,4),(8.65483889175297,12.1899094612697),
 .UNSPECIFIED.);
#196=B_SPLINE_CURVE_WITH_KNOTS('',3,(#10258,#10259,#10260,#10261),
 .UNSPECIFIED.,.F.,.F.,(4,4),(0.491886782059505,4.00844302274363),
 .UNSPECIFIED.);
#197=B_SPLINE_CURVE_WITH_KNOTS('',3,(#10264,#10265,#10266,#10267,#10268,
#10269,#10270,#10271,#10272,#10273),.UNSPECIFIED.,.F.,.F.,(4,3,3,4),(4.20909064274042,
6.3236533433415,8.26419514194387,8.41669725637478),.UNSPECIFIED.);
#198=B_SPLINE_CURVE_WITH_KNOTS('',3,(#10276,#10277,#10278,#10279),
 .UNSPECIFIED.,.F.,.F.,(4,4),(8.61714174069208,11.8187712274298),
 .UNSPECIFIED.);
#199=B_SPLINE_CURVE_WITH_KNOTS('',3,(#10283,#10284,#10285,#10286),
 .UNSPECIFIED.,.F.,.F.,(4,4),(12.0182076143484,12.6179302061492),
 .UNSPECIFIED.);
#200=B_SPLINE_CURVE_WITH_KNOTS('',3,(#10287,#10288,#10289,#10290,#10291,
#10292,#10293,#10294,#10295,#10296,#10297,#10298,#10299,#10300,#10301,#10302,
#10303,#10304,#10305,#10306,#10307,#10308,#10309,#10310,#10311,#10312,#10313,
#10314),.UNSPECIFIED.,.F.,.F.,(4,3,3,3,3,3,3,3,3,4),(0.,0.023812730958415,
0.0390943730497349,0.0628727645281949,0.0664866407211859,0.0780895647789142,
0.102003044086093,0.117056568347941,0.14081843048439,0.155095961761698),
 .UNSPECIFIED.);
#201=B_SPLINE_CURVE_WITH_KNOTS('',3,(#10318,#10319,#10320,#10321,#10322,
#10323,#10324,#10325,#10326,#10327,#10328,#10329,#10330,#10331,#10332,#10333,
#10334,#10335,#10336,#10337,#10338,#10339,#10340,#10341,#10342,#10343,#10344,
#10345,#10346,#10347,#10348,#10349,#10350,#10351,#10352,#10353,#10354),
 .UNSPECIFIED.,.F.,.F.,(4,3,3,3,3,3,3,3,3,3,3,3,4),(0.,0.0535193130531386,
0.107740084455895,0.117281563739951,0.171478196787188,0.199460035548543,
0.234266327019636,0.287962832542679,0.34249270416273,0.351167719367162,
0.408228095477446,0.46132246935065,0.46528847158773),.UNSPECIFIED.);
#202=B_SPLINE_CURVE_WITH_KNOTS('',3,(#10356,#10357,#10358,#10359),
 .UNSPECIFIED.,.F.,.F.,(4,4),(0.0221781183199723,0.974834454777906),
 .UNSPECIFIED.);
#203=B_SPLINE_CURVE_WITH_KNOTS('',3,(#10361,#10362,#10363,#10364,#10365,
#10366,#10367,#10368,#10369,#10370,#10371,#10372,#10373,#10374,#10375,#10376,
#10377,#10378,#10379,#10380,#10381,#10382,#10383,#10384,#10385,#10386,#10387,
#10388,#10389,#10390,#10391,#10392,#10393,#10394,#10395,#10396,#10397,#10398,
#10399,#10400,#10401,#10402,#10403),.UNSPECIFIED.,.F.,.F.,(4,3,3,3,3,3,
3,3,3,3,3,3,3,3,4),(0.,0.0533317239385299,0.107762434368039,0.117305236535198,
0.171635266834242,0.216430402805854,0.234303130921432,0.288010415584935,
0.341932185058889,0.351200358601802,0.360578786332496,0.414653942238971,
0.427906071157934,0.482008506259547,0.504658879840573),.UNSPECIFIED.);
#204=B_SPLINE_CURVE_WITH_KNOTS('',3,(#10407,#10408,#10409,#10410,#10411,
#10412,#10413,#10414,#10415,#10416,#10417,#10418,#10419,#10420,#10421,#10422,
#10423,#10424,#10425,#10426,#10427,#10428,#10429,#10430,#10431,#10432,#10433,
#10434,#10435,#10436,#10437,#10438,#10439,#10440,#10441,#10442,#10443,#10444,
#10445,#10446,#10447,#10448,#10449),.UNSPECIFIED.,.F.,.F.,(4,3,3,3,3,3,
3,3,3,3,3,3,3,3,4),(0.,0.0533492049661439,0.107791770949794,0.117401360885473,
0.171729175646356,0.216477851539682,0.234467324023732,0.288191829779795,
0.342104640447882,0.351366010290958,0.360619117109406,0.414688080797906,
0.427993719046535,0.482081475021072,0.504664253934307),.UNSPECIFIED.);
#205=B_SPLINE_CURVE_WITH_KNOTS('',3,(#10451,#10452,#10453,#10454),
 .UNSPECIFIED.,.F.,.F.,(4,4),(0.0251655452220943,0.977821881680028),
 .UNSPECIFIED.);
#206=B_SPLINE_CURVE_WITH_KNOTS('',3,(#10456,#10457,#10458,#10459,#10460,
#10461,#10462,#10463,#10464,#10465,#10466,#10467,#10468,#10469,#10470,#10471,
#10472,#10473,#10474,#10475,#10476,#10477,#10478,#10479,#10480,#10481,#10482,
#10483,#10484,#10485,#10486,#10487,#10488,#10489,#10490,#10491,#10492),
 .UNSPECIFIED.,.F.,.F.,(4,3,3,3,3,3,3,3,3,3,3,3,4),(0.,0.053523079491772,
0.107745541051727,0.117301531762597,0.171497090450284,0.19946878868074,
0.234298606923062,0.287998861062908,0.34252758042597,0.351197710209308,
0.408243668718811,0.4613343165756,0.465289627228313),.UNSPECIFIED.);
#207=B_SPLINE_CURVE_WITH_KNOTS('',3,(#10495,#10496,#10497,#10498,#10499,
#10500,#10501,#10502,#10503,#10504,#10505,#10506,#10507,#10508,#10509,#10510,
#10511,#10512,#10513,#10514,#10515,#10516,#10517,#10518,#10519,#10520,#10521,
#10522),.UNSPECIFIED.,.F.,.F.,(4,3,3,3,3,3,3,3,3,4),(0.,0.0238139464176845,
0.039101051769884,0.0628789982206146,0.0664894862143964,0.0781003874493316,
0.102014483019035,0.11706667068295,0.140827139970411,0.155096347075245),
 .UNSPECIFIED.);
#208=B_SPLINE_CURVE_WITH_KNOTS('',3,(#10524,#10525,#10526,#10527),
 .UNSPECIFIED.,.F.,.F.,(4,4),(2.42791692093292E-5,0.602904494019558),
 .UNSPECIFIED.);
#209=B_SPLINE_CURVE_WITH_KNOTS('',3,(#10530,#10531,#10532,#10533),
 .UNSPECIFIED.,.F.,.F.,(4,4),(0.8033909285608,4.02187648095927),
 .UNSPECIFIED.);
#210=B_SPLINE_CURVE_WITH_KNOTS('',3,(#10536,#10537,#10538,#10539,#10540,
#10541,#10542,#10543,#10544,#10545),.UNSPECIFIED.,.F.,.F.,(4,3,3,4),(4.22337623295021,
6.17414866693447,6.32726315261627,8.45313487255185),.UNSPECIFIED.);
#211=B_SPLINE_CURVE_WITH_KNOTS('',3,(#10549,#10550,#10551,#10552),
 .UNSPECIFIED.,.F.,.F.,(4,4),(12.3921295467468,12.6843586902602),
 .UNSPECIFIED.);
#212=B_SPLINE_CURVE_WITH_KNOTS('',3,(#10554,#10555,#10556,#10557,#10558,
#10559,#10560,#10561,#10562,#10563,#10564,#10565,#10566,#10567,#10568,#10569,
#10570,#10571,#10572,#10573,#10574,#10575,#10576,#10577,#10578,#10579,#10580,
#10581,#10582,#10583,#10584,#10585,#10586,#10587),.UNSPECIFIED.,.F.,.F.,
(4,3,3,3,3,3,3,3,3,3,3,4),(0.,0.0238043957114055,0.0391346151758438,0.0629652053320384,
0.0721593756253901,0.0781571886687045,0.101948185591131,0.117123476992186,
0.12020682003633,0.142665945482357,0.166389927689249,0.168222194312373),
 .UNSPECIFIED.);
#213=B_SPLINE_CURVE_WITH_KNOTS('',3,(#10591,#10592,#10593,#10594,#10595,
#10596,#10597,#10598,#10599,#10600,#10601,#10602,#10603,#10604,#10605,#10606,
#10607,#10608,#10609,#10610,#10611,#10612,#10613,#10614,#10615,#10616,#10617,
#10618,#10619,#10620,#10621,#10622,#10623,#10624),.UNSPECIFIED.,.F.,.F.,
(4,3,3,3,3,3,3,3,3,3,3,4),(0.,0.023797882907907,0.039102479174454,0.0629340675289177,
0.0721439954475325,0.0781021576199648,0.101891255326939,0.117067721419617,
0.120193732390416,0.142636523050355,0.16636673084783,0.168220399847748),
 .UNSPECIFIED.);
#214=B_SPLINE_CURVE_WITH_KNOTS('',3,(#10626,#10627,#10628,#10629),
 .UNSPECIFIED.,.F.,.F.,(4,4),(2.71213177756024E-5,0.290725780256064),
 .UNSPECIFIED.);
#215=B_SPLINE_CURVE_WITH_KNOTS('',3,(#10639,#10640,#10641,#10642,#10643,
#10644),.UNSPECIFIED.,.F.,.F.,(4,2,4),(-0.6065913737563,-0.303324265158378,
-0.00121210420063977),.UNSPECIFIED.);
#216=B_SPLINE_CURVE_WITH_KNOTS('',3,(#10646,#10647,#10648,#10649,#10650,
#10651),.UNSPECIFIED.,.F.,.F.,(4,2,4),(-0.605468679705391,-0.303324901248498,
-8.9425867424664E-5),.UNSPECIFIED.);
#217=B_SPLINE_CURVE_WITH_KNOTS('',3,(#10653,#10654,#10655,#10656,#10657,
#10658,#10659,#10660,#10661,#10662,#10663,#10664,#10665,#10666,#10667,#10668,
#10669,#10670,#10671,#10672,#10673,#10674,#10675,#10676,#10677,#10678,#10679,
#10680),.UNSPECIFIED.,.F.,.F.,(4,3,3,3,3,3,3,3,3,4),(-0.153261590805415,
-0.129427422483982,-0.117093626371441,-0.093122524304512,-0.077863059046492,
-0.0655799937729104,-0.0417579003169496,-0.0388648221790391,-0.0150894148558222,
0.),.UNSPECIFIED.);
#218=B_SPLINE_CURVE_WITH_KNOTS('',3,(#10683,#10684,#10685,#10686,#10687,
#10688,#10689,#10690,#10691,#10692,#10693,#10694,#10695,#10696,#10697,#10698,
#10699,#10700,#10701,#10702,#10703,#10704,#10705,#10706,#10707,#10708,#10709,
#10710),.UNSPECIFIED.,.F.,.F.,(4,3,3,3,3,3,3,3,3,4),(-0.153296867786173,
-0.129546774976449,-0.118009772088948,-0.0941871764575653,-0.08771862273971,
-0.0788646444725944,-0.0549216410880561,-0.0394902966566095,-0.0156128557692252,
0.),.UNSPECIFIED.);
#219=B_SPLINE_CURVE_WITH_KNOTS('',3,(#10727,#10728,#10729,#10730),
 .UNSPECIFIED.,.F.,.F.,(4,4),(-4.3123055228435,-0.796205213256333),
 .UNSPECIFIED.);
#220=B_SPLINE_CURVE_WITH_KNOTS('',3,(#10748,#10749,#10750,#10751),
 .UNSPECIFIED.,.F.,.F.,(4,4),(-0.594853877716395,-0.335767855111383),
 .UNSPECIFIED.);
#221=B_SPLINE_CURVE_WITH_KNOTS('',3,(#10752,#10753,#10754,#10755),
 .UNSPECIFIED.,.F.,.F.,(4,4),(-0.615688454110788,-0.00935595183171186),
 .UNSPECIFIED.);
#222=B_SPLINE_CURVE_WITH_KNOTS('',3,(#10776,#10777,#10778,#10779),
 .UNSPECIFIED.,.F.,.F.,(4,4),(0.806548880270408,4.31873271634551),
 .UNSPECIFIED.);
#223=B_SPLINE_CURVE_WITH_KNOTS('',3,(#10801,#10802,#10803,#10804),
 .UNSPECIFIED.,.F.,.F.,(4,4),(0.335767855111383,0.605460332260614),
 .UNSPECIFIED.);
#224=B_SPLINE_CURVE_WITH_KNOTS('',3,(#10807,#10808,#10809,#10810),
 .UNSPECIFIED.,.F.,.F.,(4,4),(8.8675541747208,12.379738010796),
 .UNSPECIFIED.);
#225=B_SPLINE_CURVE_WITH_KNOTS('',3,(#10813,#10814,#10815,#10816),
 .UNSPECIFIED.,.F.,.F.,(4,4),(12.5808265588057,12.8505190359549),
 .UNSPECIFIED.);
#226=B_SPLINE_CURVE_WITH_KNOTS('',3,(#10838,#10839,#10840,#10841),
 .UNSPECIFIED.,.F.,.F.,(4,4),(-12.3900816778099,-8.87398136822274),
 .UNSPECIFIED.);
#227=B_SPLINE_CURVE_WITH_KNOTS('',3,(#10875,#10876,#10877,#10878),
 .UNSPECIFIED.,.F.,.F.,(4,4),(0.00935595183171174,0.615688454110787),
 .UNSPECIFIED.);
#228=B_SPLINE_CURVE_WITH_KNOTS('',3,(#10879,#10880,#10881,#10882),
 .UNSPECIFIED.,.F.,.F.,(4,4),(-12.8505190359549,-12.5914330133498),
 .UNSPECIFIED.);
#229=B_SPLINE_CURVE_WITH_KNOTS('',3,(#10885,#10886,#10887,#10888,#10889,
#10890),.UNSPECIFIED.,.F.,.F.,(4,2,4),(-0.606830654194234,-0.303665168982051,
-0.00091389508118378),.UNSPECIFIED.);
#230=B_SPLINE_CURVE_WITH_KNOTS('',3,(#10892,#10893,#10894,#10895,#10896,
#10897,#10898,#10899,#10900,#10901,#10902,#10903,#10904,#10905,#10906,#10907,
#10908,#10909,#10910,#10911,#10912,#10913,#10914,#10915,#10916,#10917,#10918,
#10919),.UNSPECIFIED.,.F.,.F.,(4,3,3,3,3,3,3,3,3,4),(-0.152562937837783,
-0.12881903955137,-0.117160811640917,-0.0932181166800446,-0.0780374575565173,
-0.0653603882662585,-0.0415602279441365,-0.0389951227734853,-0.0152093108541457,
0.),.UNSPECIFIED.);
#231=B_SPLINE_CURVE_WITH_KNOTS('',3,(#10923,#10924,#10925,#10926,#10927,
#10928,#10929,#10930,#10931,#10932,#10933,#10934,#10935,#10936,#10937,#10938,
#10939,#10940,#10941,#10942,#10943,#10944,#10945,#10946,#10947,#10948,#10949,
#10950),.UNSPECIFIED.,.F.,.F.,(4,3,3,3,3,3,3,3,3,4),(-0.152573286042523,
-0.128801685906155,-0.115487540236632,-0.091707628219999,-0.0872268515824704,
-0.07838422198738,-0.0544695788315335,-0.0392121213631617,-0.0154211067806385,
0.),.UNSPECIFIED.);
#232=B_SPLINE_CURVE_WITH_KNOTS('',3,(#10951,#10952,#10953,#10954,#10955,
#10956),.UNSPECIFIED.,.F.,.F.,(4,2,4),(-0.606417229744719,-0.30366508312326,
-0.000500462001714608),.UNSPECIFIED.);
#233=B_SPLINE_CURVE_WITH_KNOTS('',3,(#10973,#10974,#10975,#10976),
 .UNSPECIFIED.,.F.,.F.,(4,4),(-8.7204856127415,-4.5128966022766),
 .UNSPECIFIED.);
#234=B_SPLINE_CURVE_WITH_KNOTS('',3,(#10997,#10998,#10999,#11000),
 .UNSPECIFIED.,.F.,.F.,(4,4),(4.51913891174751,8.72381854299666),
 .UNSPECIFIED.);
#235=B_SPLINE_CURVE_WITH_KNOTS('',3,(#11002,#11003,#11004,#11005),
 .UNSPECIFIED.,.F.,.F.,(4,4),(4.46246834806959,8.66714797931881),
 .UNSPECIFIED.);
#236=B_SPLINE_CURVE_WITH_KNOTS('',3,(#11026,#11027,#11028,#11029),
 .UNSPECIFIED.,.F.,.F.,(4,4),(-8.67339028878965,-4.46580127832475),
 .UNSPECIFIED.);
#237=B_SPLINE_CURVE_WITH_KNOTS('',3,(#11048,#11049,#11050,#11051,#11052,
#11053),.UNSPECIFIED.,.F.,.F.,(4,2,4),(-0.607391644691745,-0.303762155877002,
-0.00125172564267001),.UNSPECIFIED.);
#238=B_SPLINE_CURVE_WITH_KNOTS('',3,(#11054,#11055,#11056,#11057,#11058,
#11059,#11060,#11061,#11062,#11063,#11064,#11065,#11066,#11067,#11068,#11069,
#11070,#11071,#11072,#11073,#11074,#11075,#11076,#11077,#11078,#11079,#11080,
#11081),.UNSPECIFIED.,.F.,.F.,(4,3,3,3,3,3,3,3,3,4),(-0.152281539067936,
-0.12854821222061,-0.115190816126163,-0.0912758856104041,-0.0781043161616985,
-0.0652713841318381,-0.0414808619979686,-0.039045740680325,-0.0152551599791835,
0.),.UNSPECIFIED.);
#239=B_SPLINE_CURVE_WITH_KNOTS('',3,(#11083,#11084,#11085,#11086,#11087,
#11088,#11089,#11090,#11091,#11092,#11093,#11094,#11095,#11096,#11097,#11098,
#11099,#11100,#11101,#11102,#11103,#11104,#11105,#11106,#11107,#11108,#11109,
#11110),.UNSPECIFIED.,.F.,.F.,(4,3,3,3,3,3,3,3,3,4),(-0.152284734818265,
-0.128510300097745,-0.115243636037359,-0.0914764658269932,-0.0870316758632336,
-0.078197793898112,-0.0542955901223581,-0.0391042908842167,-0.0153462458625635,
0.),.UNSPECIFIED.);
#240=B_SPLINE_CURVE_WITH_KNOTS('',3,(#11111,#11112,#11113,#11114,#11115,
#11116),.UNSPECIFIED.,.F.,.F.,(4,2,4),(-0.606273164239037,-0.303762187833104,
-0.000133245189939568),.UNSPECIFIED.);
#241=B_SPLINE_CURVE_WITH_KNOTS('',3,(#11133,#11134,#11135,#11136),
 .UNSPECIFIED.,.F.,.F.,(4,4),(-12.1227852464729,-8.92068531110742),
 .UNSPECIFIED.);
#242=B_SPLINE_CURVE_WITH_KNOTS('',3,(#11177,#11178,#11179,#11180),
 .UNSPECIFIED.,.F.,.F.,(4,4),(-4.26560157995882,-1.06350164459338),
 .UNSPECIFIED.);
#243=B_SPLINE_CURVE_WITH_KNOTS('',3,(#11199,#11200,#11201,#11202,#11203,
#11204),.UNSPECIFIED.,.F.,.F.,(4,2,4),(-0.607545900263938,-0.303784727094449,
-0.00134539382494125),.UNSPECIFIED.);
#244=B_SPLINE_CURVE_WITH_KNOTS('',3,(#11206,#11207,#11208,#11209,#11210,
#11211,#11212,#11213,#11214,#11215,#11216,#11217,#11218,#11219,#11220,#11221,
#11222,#11223,#11224,#11225,#11226,#11227,#11228,#11229,#11230,#11231,#11232,
#11233),.UNSPECIFIED.,.F.,.F.,(4,3,3,3,3,3,3,3,3,4),(-0.152214473108837,
-0.128485298747135,-0.115164309990209,-0.0912534321321267,-0.0781163092888813,
-0.0652482412471129,-0.0414606388666645,-0.0390548598067502,-0.0152611452145655,
0.),.UNSPECIFIED.);
#245=B_SPLINE_CURVE_WITH_KNOTS('',3,(#11237,#11238,#11239,#11240,#11241,
#11242,#11243,#11244,#11245,#11246,#11247,#11248,#11249,#11250,#11251,#11252,
#11253,#11254,#11255,#11256,#11257,#11258,#11259,#11260,#11261,#11262,#11263,
#11264),.UNSPECIFIED.,.F.,.F.,(4,3,3,3,3,3,3,3,3,4),(-0.152216110966007,
-0.128438825687404,-0.115191384846861,-0.0914281188167518,-0.0869870566155827,
-0.0781642271790374,-0.0542662950786889,-0.0390848818783988,-0.0153309789665,
0.),.UNSPECIFIED.);
#246=B_SPLINE_CURVE_WITH_KNOTS('',3,(#11265,#11266,#11267,#11268,#11269,
#11270),.UNSPECIFIED.,.F.,.F.,(4,2,4),(-0.606227037063105,-0.303784766192107,
-2.65251918123988E-5),.UNSPECIFIED.);
#247=B_SPLINE_CURVE_WITH_KNOTS('',3,(#11288,#11289,#11290,#11291),
 .UNSPECIFIED.,.F.,.F.,(4,4),(0.0107208554739345,0.617725317592517),
 .UNSPECIFIED.);
#248=B_SPLINE_CURVE_WITH_KNOTS('',3,(#11292,#11293,#11294,#11295),
 .UNSPECIFIED.,.F.,.F.,(4,4),(-12.893479658151,-12.3228618033436),
 .UNSPECIFIED.);
#249=B_SPLINE_CURVE_WITH_KNOTS('',3,(#11318,#11319,#11320,#11321),
 .UNSPECIFIED.,.F.,.F.,(4,4),(12.3251818525939,12.893479658151),
 .UNSPECIFIED.);
#250=B_SPLINE_CURVE_WITH_KNOTS('',3,(#11325,#11326,#11327,#11328),
 .UNSPECIFIED.,.F.,.F.,(4,4),(0.292807233425235,0.861105038472338),
 .UNSPECIFIED.);
#251=B_SPLINE_CURVE_WITH_KNOTS('',3,(#11346,#11347,#11348,#11349),
 .UNSPECIFIED.,.F.,.F.,(4,4),(-0.863425087722636,-0.29280723291527),
 .UNSPECIFIED.);
#252=B_SPLINE_CURVE_WITH_KNOTS('',3,(#11350,#11351,#11352,#11353),
 .UNSPECIFIED.,.F.,.F.,(4,4),(-0.617725317592517,-0.0107208554739345),
 .UNSPECIFIED.);
#253=B_SPLINE_CURVE_WITH_KNOTS('',3,(#11437,#11438,#11439,#11440),
 .UNSPECIFIED.,.F.,.F.,(4,4),(0.00878563933291533,0.615688454110788),
 .UNSPECIFIED.);
#254=B_SPLINE_CURVE_WITH_KNOTS('',3,(#11465,#11466,#11467,#11468),
 .UNSPECIFIED.,.F.,.F.,(4,4),(-0.615688454110787,-0.00878563933291527),
 .UNSPECIFIED.);
#255=B_SPLINE_CURVE_WITH_KNOTS('',3,(#11554,#11555,#11556,#11557),
 .UNSPECIFIED.,.F.,.F.,(4,4),(-9.62771529167128E-17,0.617725317592517),
 .UNSPECIFIED.);
#256=B_SPLINE_CURVE_WITH_KNOTS('',3,(#11558,#11559,#11560,#11561),
 .UNSPECIFIED.,.F.,.F.,(4,4),(-0.617725317592517,-0.000337488966422091),
 .UNSPECIFIED.);
#257=B_SPLINE_CURVE_WITH_KNOTS('',3,(#11597,#11598,#11599,#11600,#11601),
 .UNSPECIFIED.,.F.,.F.,(4,1,4),(-12.893479658151,-5.71764434212835,-0.335767855111383),
 .UNSPECIFIED.);
#258=B_SPLINE_CURVE_WITH_KNOTS('',3,(#11602,#11603,#11604,#11605,#11606),
 .UNSPECIFIED.,.F.,.F.,(4,1,4),(0.335767855111383,5.71764434212835,12.893479658151),
 .UNSPECIFIED.);
#259=B_SPLINE_CURVE_WITH_KNOTS('',3,(#11631,#11632,#11633,#11634),
 .UNSPECIFIED.,.F.,.F.,(4,4),(-0.00171041937131743,0.615688454110788),
 .UNSPECIFIED.);
#260=B_SPLINE_CURVE_WITH_KNOTS('',3,(#11635,#11636,#11637,#11638),
 .UNSPECIFIED.,.F.,.F.,(4,4),(-0.615688454110788,-3.98826847727851E-7),
 .UNSPECIFIED.);
#261=B_SPLINE_CURVE_WITH_KNOTS('',3,(#11663,#11664,#11665,#11666),
 .UNSPECIFIED.,.F.,.F.,(4,4),(3.98826847219577E-7,0.615688454110787),
 .UNSPECIFIED.);
#262=B_SPLINE_CURVE_WITH_KNOTS('',3,(#11667,#11668,#11669,#11670),
 .UNSPECIFIED.,.F.,.F.,(4,4),(-0.615688454110787,0.0017104193713176),
 .UNSPECIFIED.);
#263=B_SPLINE_CURVE_WITH_KNOTS('',3,(#11696,#11697,#11698,#11699,#11700),
 .UNSPECIFIED.,.F.,.F.,(4,1,4),(-12.8505190359549,-7.4686425489379,-0.29280723291527),
 .UNSPECIFIED.);
#264=B_SPLINE_CURVE_WITH_KNOTS('',3,(#11701,#11702,#11703,#11704,#11705),
 .UNSPECIFIED.,.F.,.F.,(4,1,4),(0.292807233425236,7.4686425489379,12.8505190359549),
 .UNSPECIFIED.);
#265=B_SPLINE_CURVE_WITH_KNOTS('',3,(#11726,#11727,#11728,#11729),
 .UNSPECIFIED.,.F.,.F.,(4,4),(0.000337488966421928,0.617725317592517),
 .UNSPECIFIED.);
#266=B_SPLINE_CURVE_WITH_KNOTS('',3,(#11730,#11731,#11732,#11733),
 .UNSPECIFIED.,.F.,.F.,(4,4),(-0.617725317592517,8.06646416329215E-17),
 .UNSPECIFIED.);
#267=B_SPLINE_CURVE_WITH_KNOTS('',3,(#11773,#11774,#11775,#11776),
 .UNSPECIFIED.,.F.,.F.,(4,4),(3.28016616408593,4.26236080300681),
 .UNSPECIFIED.);
#268=B_SPLINE_CURVE_WITH_KNOTS('',3,(#11780,#11781,#11782,#11783),
 .UNSPECIFIED.,.F.,.F.,(4,4),(8.92392608805945,9.90612072688831),
 .UNSPECIFIED.);
#269=B_SPLINE_CURVE_WITH_KNOTS('',3,(#11785,#11786,#11787,#11788,#11789,
#11790,#11791,#11792,#11793,#11794,#11795,#11796,#11797,#11798,#11799,#11800,
#11801,#11802,#11803),.UNSPECIFIED.,.F.,.F.,(4,3,3,3,3,3,4),(-0.050768112872884,
-0.0388528786649772,-0.0311058171716578,-0.0259830388669653,-0.0210744122964195,
-0.0143837148934404,0.),.UNSPECIFIED.);
#270=B_SPLINE_CURVE_WITH_KNOTS('',3,(#11805,#11806,#11807,#11808),
 .UNSPECIFIED.,.F.,.F.,(4,4),(9.9568018127159,12.1251256661408),
 .UNSPECIFIED.);
#271=B_SPLINE_CURVE_WITH_KNOTS('',3,(#11812,#11813,#11814,#11815),
 .UNSPECIFIED.,.F.,.F.,(4,4),(1.06116122492545,3.22948508825557),
 .UNSPECIFIED.);
#272=B_SPLINE_CURVE_WITH_KNOTS('',3,(#11816,#11817,#11818,#11819,#11820,
#11821,#11822,#11823,#11824,#11825,#11826,#11827,#11828,#11829,#11830,#11831,
#11832,#11833,#11834),.UNSPECIFIED.,.F.,.F.,(4,3,3,3,3,3,4),(-0.0507681129736439,
-0.0388528772897764,-0.0311058147321604,-0.0259830361493327,-0.0210744097201194,
-0.0143837130754026,-9.90506278315E-9),.UNSPECIFIED.);
#273=B_SPLINE_CURVE_WITH_KNOTS('',3,(#12042,#12043,#12044,#12045,#12046,
#12047),.UNSPECIFIED.,.F.,.F.,(4,2,4),(-0.605566356596631,-0.303329629920269,
-0.000148729590407126),.UNSPECIFIED.);
#274=B_SPLINE_CURVE_WITH_KNOTS('',3,(#12049,#12050,#12051,#12052,#12053,
#12054,#12055,#12056,#12057,#12058,#12059,#12060,#12061,#12062,#12063,#12064,
#12065,#12066,#12067,#12068,#12069,#12070,#12071,#12072,#12073,#12074,#12075,
#12076),.UNSPECIFIED.,.F.,.F.,(4,3,3,3,3,3,3,3,3,4),(-0.153210533292091,
-0.129383071834804,-0.117098895005168,-0.0931297672424715,-0.0778761857300216,
-0.065564095006876,-0.0417435583396367,-0.038874550231651,-0.0150983388519663,
0.),.UNSPECIFIED.);
#275=B_SPLINE_CURVE_WITH_KNOTS('',3,(#12080,#12081,#12082,#12083,#12084,
#12085,#12086,#12087,#12088,#12089,#12090,#12091,#12092,#12093,#12094,#12095,
#12096,#12097,#12098,#12099,#12100,#12101,#12102,#12103,#12104,#12105,#12106,
#12107),.UNSPECIFIED.,.F.,.F.,(4,3,3,3,3,3,3,3,3,4),(-0.153244081227051,
-0.129493605146206,-0.117970006482883,-0.0941492904140308,-0.0876825809854227,
-0.078828741443105,-0.0548877675055393,-0.0394694906046094,-0.0155984926894347,
0.),.UNSPECIFIED.);
#276=B_SPLINE_CURVE_WITH_KNOTS('',3,(#12108,#12109,#12110,#12111,#12112,
#12113),.UNSPECIFIED.,.F.,.F.,(4,2,4),(-0.606539490527658,-0.303329031627741,
-0.00112184825655631),.UNSPECIFIED.);
#277=B_SPLINE_CURVE_WITH_KNOTS('',3,(#12118,#12119,#12120,#12121,#12122,
#12123),.UNSPECIFIED.,.F.,.F.,(4,2,4),(-0.606785247764818,-0.303663188081886,
-0.00088649083675002),.UNSPECIFIED.);
#278=B_SPLINE_CURVE_WITH_KNOTS('',3,(#12125,#12126,#12127,#12128,#12129,
#12130,#12131,#12132,#12133,#12134,#12135,#12136,#12137,#12138,#12139,#12140,
#12141,#12142,#12143,#12144,#12145,#12146,#12147,#12148,#12149,#12150,#12151,
#12152),.UNSPECIFIED.,.F.,.F.,(4,3,3,3,3,3,3,3,3,4),(-0.15258577077829,
-0.128839317352572,-0.117158786685373,-0.0932148261566644,-0.0780319390000633,
-0.0653676349965338,-0.0415665498371782,-0.0389909618069961,-0.0152059030050533,
0.),.UNSPECIFIED.);
#279=B_SPLINE_CURVE_WITH_KNOTS('',3,(#12156,#12157,#12158,#12159,#12160,
#12161,#12162,#12163,#12164,#12165,#12166,#12167,#12168,#12169,#12170,#12171,
#12172,#12173,#12174,#12175,#12176,#12177,#12178,#12179,#12180,#12181,#12182,
#12183),.UNSPECIFIED.,.F.,.F.,(4,3,3,3,3,3,3,3,3,4),(-0.152596853546747,
-0.128825864440686,-0.115507515430042,-0.0917263797372463,-0.0872428123353572,
-0.0783995504057471,-0.0544835945915644,-0.0392209901554083,-0.0154275313391792,
0.),.UNSPECIFIED.);
#280=B_SPLINE_CURVE_WITH_KNOTS('',3,(#12185,#12186,#12187,#12188,#12189,
#12190),.UNSPECIFIED.,.F.,.F.,(4,2,4),(-0.606440835737524,-0.303663090452391,
-0.000542069086802599),.UNSPECIFIED.);
#281=B_SPLINE_CURVE_WITH_KNOTS('',3,(#12196,#12197,#12198,#12199,#12200,
#12201),.UNSPECIFIED.,.F.,.F.,(4,2,4),(-0.607379220946441,-0.303761646676304,
-0.00124422999587004),.UNSPECIFIED.);
#282=B_SPLINE_CURVE_WITH_KNOTS('',3,(#12203,#12204,#12205,#12206,#12207,
#12208,#12209,#12210,#12211,#12212,#12213,#12214,#12215,#12216,#12217,#12218,
#12219,#12220,#12221,#12222,#12223,#12224,#12225,#12226,#12227,#12228,#12229,
#12230),.UNSPECIFIED.,.F.,.F.,(4,3,3,3,3,3,3,3,3,4),(-0.152287640102895,
-0.128554450486317,-0.115193035178751,-0.0912770810520543,-0.0781028969167454,
-0.0652733399726575,-0.0414820896655672,-0.0390446621366508,-0.0152552334863041,
0.),.UNSPECIFIED.);
#283=B_SPLINE_CURVE_WITH_KNOTS('',3,(#12234,#12235,#12236,#12237,#12238,
#12239,#12240,#12241,#12242,#12243,#12244,#12245,#12246,#12247,#12248,#12249,
#12250,#12251,#12252,#12253,#12254,#12255,#12256,#12257,#12258,#12259,#12260,
#12261),.UNSPECIFIED.,.F.,.F.,(4,3,3,3,3,3,3,3,3,4),(-0.152291020205185,
-0.128517753946702,-0.115248901231919,-0.0914807886786037,-0.0870359119466785,
-0.0782017654295232,-0.054298407767766,-0.03910658747416,-0.0153486482327859,
0.),.UNSPECIFIED.);
#284=B_SPLINE_CURVE_WITH_KNOTS('',3,(#12263,#12264,#12265,#12266,#12267,
#12268),.UNSPECIFIED.,.F.,.F.,(4,2,4),(-0.606279550122448,-0.303761677523001,
-0.000144559171857295),.UNSPECIFIED.);
#285=B_SPLINE_CURVE_WITH_KNOTS('',3,(#12274,#12275,#12276,#12277,#12278,
#12279),.UNSPECIFIED.,.F.,.F.,(4,2,4),(-0.607536685592867,-0.303784463250135,
-0.00133982193348342),.UNSPECIFIED.);
#286=B_SPLINE_CURVE_WITH_KNOTS('',3,(#12280,#12281,#12282,#12283,#12284,
#12285,#12286,#12287,#12288,#12289,#12290,#12291,#12292,#12293,#12294,#12295,
#12296,#12297,#12298,#12299,#12300,#12301,#12302,#12303,#12304,#12305,#12306,
#12307),.UNSPECIFIED.,.F.,.F.,(4,3,3,3,3,3,3,3,3,4),(-0.152217684890348,
-0.128490376540845,-0.11516578527262,-0.091253137134092,-0.0781160865160423,
-0.0652495101170982,-0.0414606291875136,-0.0390546905501479,-0.015263466236765,
0.),.UNSPECIFIED.);
#287=B_SPLINE_CURVE_WITH_KNOTS('',3,(#12309,#12310,#12311,#12312,#12313,
#12314,#12315,#12316,#12317,#12318,#12319,#12320,#12321,#12322,#12323,#12324,
#12325,#12326,#12327,#12328,#12329,#12330,#12331,#12332,#12333,#12334,#12335,
#12336),.UNSPECIFIED.,.F.,.F.,(4,3,3,3,3,3,3,3,3,4),(-0.152219351639196,
-0.128444680332832,-0.115193337419806,-0.0914284185691762,-0.0869890032859244,
-0.0781648487722283,-0.0542647883944502,-0.0390852411900305,-0.0153331469286526,
0.),.UNSPECIFIED.);
#288=B_SPLINE_CURVE_WITH_KNOTS('',3,(#12338,#12339,#12340,#12341,#12342,
#12343),.UNSPECIFIED.,.F.,.F.,(4,2,4),(-0.606231877025315,-0.303784501204342,
-3.50089943914611E-5),.UNSPECIFIED.);
#289=B_SPLINE_CURVE_WITH_KNOTS('',3,(#12349,#12350,#12351,#12352),
 .UNSPECIFIED.,.F.,.F.,(4,4),(0.0108333608245492,0.617725317592517),
 .UNSPECIFIED.);
#290=B_SPLINE_CURVE_WITH_KNOTS('',3,(#12356,#12357,#12358,#12359),
 .UNSPECIFIED.,.F.,.F.,(4,4),(-0.617725317592517,-0.0108333608245492),
 .UNSPECIFIED.);
#291=B_SPLINE_CURVE_WITH_KNOTS('',3,(#12362,#12363,#12364,#12365),
 .UNSPECIFIED.,.F.,.F.,(4,4),(8.65483889175297,12.1899094612697),
 .UNSPECIFIED.);
#292=B_SPLINE_CURVE_WITH_KNOTS('',3,(#12366,#12367,#12368,#12369),
 .UNSPECIFIED.,.F.,.F.,(4,4),(0.491886782059505,4.00844302274363),
 .UNSPECIFIED.);
#293=B_SPLINE_CURVE_WITH_KNOTS('',3,(#12372,#12373,#12374,#12375,#12376,
#12377,#12378,#12379,#12380,#12381),.UNSPECIFIED.,.F.,.F.,(4,3,3,4),(4.20909064274042,
6.3236533433415,8.26419514194387,8.41669725637478),.UNSPECIFIED.);
#294=B_SPLINE_CURVE_WITH_KNOTS('',3,(#12384,#12385,#12386,#12387),
 .UNSPECIFIED.,.F.,.F.,(4,4),(8.61714174069208,11.8187712274298),
 .UNSPECIFIED.);
#295=B_SPLINE_CURVE_WITH_KNOTS('',3,(#12391,#12392,#12393,#12394),
 .UNSPECIFIED.,.F.,.F.,(4,4),(12.0182076143484,12.6179302061492),
 .UNSPECIFIED.);
#296=B_SPLINE_CURVE_WITH_KNOTS('',3,(#12395,#12396,#12397,#12398,#12399,
#12400,#12401,#12402,#12403,#12404,#12405,#12406,#12407,#12408,#12409,#12410,
#12411,#12412,#12413,#12414,#12415,#12416,#12417,#12418,#12419,#12420,#12421,
#12422),.UNSPECIFIED.,.F.,.F.,(4,3,3,3,3,3,3,3,3,4),(0.,0.023812730958415,
0.0390943730497349,0.0628727645281949,0.0664866407211859,0.0780895647789142,
0.102003044086093,0.117056568347941,0.14081843048439,0.155095961761698),
 .UNSPECIFIED.);
#297=B_SPLINE_CURVE_WITH_KNOTS('',3,(#12426,#12427,#12428,#12429,#12430,
#12431,#12432,#12433,#12434,#12435,#12436,#12437,#12438,#12439,#12440,#12441,
#12442,#12443,#12444,#12445,#12446,#12447,#12448,#12449,#12450,#12451,#12452,
#12453,#12454,#12455,#12456,#12457,#12458,#12459,#12460,#12461,#12462),
 .UNSPECIFIED.,.F.,.F.,(4,3,3,3,3,3,3,3,3,3,3,3,4),(0.,0.0535193130531386,
0.107740084455895,0.117281563739951,0.171478196787188,0.199460035548543,
0.234266327019636,0.287962832542679,0.34249270416273,0.351167719367162,
0.408228095477446,0.46132246935065,0.46528847158773),.UNSPECIFIED.);
#298=B_SPLINE_CURVE_WITH_KNOTS('',3,(#12464,#12465,#12466,#12467),
 .UNSPECIFIED.,.F.,.F.,(4,4),(0.0221781183199723,0.974834454777906),
 .UNSPECIFIED.);
#299=B_SPLINE_CURVE_WITH_KNOTS('',3,(#12469,#12470,#12471,#12472,#12473,
#12474,#12475,#12476,#12477,#12478,#12479,#12480,#12481,#12482,#12483,#12484,
#12485,#12486,#12487,#12488,#12489,#12490,#12491,#12492,#12493,#12494,#12495,
#12496,#12497,#12498,#12499,#12500,#12501,#12502,#12503,#12504,#12505,#12506,
#12507,#12508,#12509,#12510,#12511),.UNSPECIFIED.,.F.,.F.,(4,3,3,3,3,3,
3,3,3,3,3,3,3,3,4),(0.,0.0533317239385299,0.107762434368039,0.117305236535198,
0.171635266834242,0.216430402805854,0.234303130921432,0.288010415584935,
0.341932185058889,0.351200358601802,0.360578786332496,0.414653942238971,
0.427906071157934,0.482008506259547,0.504658879840573),.UNSPECIFIED.);
#300=B_SPLINE_CURVE_WITH_KNOTS('',3,(#12515,#12516,#12517,#12518,#12519,
#12520,#12521,#12522,#12523,#12524,#12525,#12526,#12527,#12528,#12529,#12530,
#12531,#12532,#12533,#12534,#12535,#12536,#12537,#12538,#12539,#12540,#12541,
#12542,#12543,#12544,#12545,#12546,#12547,#12548,#12549,#12550,#12551,#12552,
#12553,#12554,#12555,#12556,#12557),.UNSPECIFIED.,.F.,.F.,(4,3,3,3,3,3,
3,3,3,3,3,3,3,3,4),(0.,0.0533492049661439,0.107791770949794,0.117401360885473,
0.171729175646356,0.216477851539682,0.234467324023732,0.288191829779795,
0.342104640447882,0.351366010290958,0.360619117109406,0.414688080797906,
0.427993719046535,0.482081475021072,0.504664253934307),.UNSPECIFIED.);
#301=B_SPLINE_CURVE_WITH_KNOTS('',3,(#12559,#12560,#12561,#12562),
 .UNSPECIFIED.,.F.,.F.,(4,4),(0.0251655452220943,0.977821881680028),
 .UNSPECIFIED.);
#302=B_SPLINE_CURVE_WITH_KNOTS('',3,(#12564,#12565,#12566,#12567,#12568,
#12569,#12570,#12571,#12572,#12573,#12574,#12575,#12576,#12577,#12578,#12579,
#12580,#12581,#12582,#12583,#12584,#12585,#12586,#12587,#12588,#12589,#12590,
#12591,#12592,#12593,#12594,#12595,#12596,#12597,#12598,#12599,#12600),
 .UNSPECIFIED.,.F.,.F.,(4,3,3,3,3,3,3,3,3,3,3,3,4),(0.,0.053523079491772,
0.107745541051727,0.117301531762597,0.171497090450284,0.19946878868074,
0.234298606923062,0.287998861062908,0.34252758042597,0.351197710209308,
0.408243668718811,0.4613343165756,0.465289627228313),.UNSPECIFIED.);
#303=B_SPLINE_CURVE_WITH_KNOTS('',3,(#12603,#12604,#12605,#12606,#12607,
#12608,#12609,#12610,#12611,#12612,#12613,#12614,#12615,#12616,#12617,#12618,
#12619,#12620,#12621,#12622,#12623,#12624,#12625,#12626,#12627,#12628,#12629,
#12630),.UNSPECIFIED.,.F.,.F.,(4,3,3,3,3,3,3,3,3,4),(0.,0.0238139464176845,
0.039101051769884,0.0628789982206146,0.0664894862143964,0.0781003874493316,
0.102014483019035,0.11706667068295,0.140827139970411,0.155096347075245),
 .UNSPECIFIED.);
#304=B_SPLINE_CURVE_WITH_KNOTS('',3,(#12632,#12633,#12634,#12635),
 .UNSPECIFIED.,.F.,.F.,(4,4),(2.42791692093292E-5,0.602904494019558),
 .UNSPECIFIED.);
#305=B_SPLINE_CURVE_WITH_KNOTS('',3,(#12638,#12639,#12640,#12641),
 .UNSPECIFIED.,.F.,.F.,(4,4),(0.8033909285608,4.02187648095927),
 .UNSPECIFIED.);
#306=B_SPLINE_CURVE_WITH_KNOTS('',3,(#12644,#12645,#12646,#12647,#12648,
#12649,#12650,#12651,#12652,#12653),.UNSPECIFIED.,.F.,.F.,(4,3,3,4),(4.22337623295021,
6.17414866693447,6.32726315261627,8.45313487255185),.UNSPECIFIED.);
#307=B_SPLINE_CURVE_WITH_KNOTS('',3,(#12657,#12658,#12659,#12660),
 .UNSPECIFIED.,.F.,.F.,(4,4),(12.3921295467468,12.6843586902602),
 .UNSPECIFIED.);
#308=B_SPLINE_CURVE_WITH_KNOTS('',3,(#12662,#12663,#12664,#12665,#12666,
#12667,#12668,#12669,#12670,#12671,#12672,#12673,#12674,#12675,#12676,#12677,
#12678,#12679,#12680,#12681,#12682,#12683,#12684,#12685,#12686,#12687,#12688,
#12689,#12690,#12691,#12692,#12693,#12694,#12695),.UNSPECIFIED.,.F.,.F.,
(4,3,3,3,3,3,3,3,3,3,3,4),(0.,0.0238043957114055,0.0391346151758438,0.0629652053320384,
0.0721593756253901,0.0781571886687045,0.101948185591131,0.117123476992186,
0.12020682003633,0.142665945482357,0.166389927689249,0.168222194312373),
 .UNSPECIFIED.);
#309=B_SPLINE_CURVE_WITH_KNOTS('',3,(#12699,#12700,#12701,#12702,#12703,
#12704,#12705,#12706,#12707,#12708,#12709,#12710,#12711,#12712,#12713,#12714,
#12715,#12716,#12717,#12718,#12719,#12720,#12721,#12722,#12723,#12724,#12725,
#12726,#12727,#12728,#12729,#12730,#12731,#12732),.UNSPECIFIED.,.F.,.F.,
(4,3,3,3,3,3,3,3,3,3,3,4),(0.,0.023797882907907,0.039102479174454,0.0629340675289177,
0.0721439954475325,0.0781021576199648,0.101891255326939,0.117067721419617,
0.120193732390416,0.142636523050355,0.16636673084783,0.168220399847748),
 .UNSPECIFIED.);
#310=B_SPLINE_CURVE_WITH_KNOTS('',3,(#12734,#12735,#12736,#12737),
 .UNSPECIFIED.,.F.,.F.,(4,4),(2.71213177756024E-5,0.290725780256064),
 .UNSPECIFIED.);
#311=B_SPLINE_CURVE_WITH_KNOTS('',3,(#12747,#12748,#12749,#12750,#12751,
#12752),.UNSPECIFIED.,.F.,.F.,(4,2,4),(-0.6065913737563,-0.303324265158378,
-0.00121210420063977),.UNSPECIFIED.);
#312=B_SPLINE_CURVE_WITH_KNOTS('',3,(#12754,#12755,#12756,#12757,#12758,
#12759),.UNSPECIFIED.,.F.,.F.,(4,2,4),(-0.605468679705391,-0.303324901248498,
-8.9425867424664E-5),.UNSPECIFIED.);
#313=B_SPLINE_CURVE_WITH_KNOTS('',3,(#12761,#12762,#12763,#12764,#12765,
#12766,#12767,#12768,#12769,#12770,#12771,#12772,#12773,#12774,#12775,#12776,
#12777,#12778,#12779,#12780,#12781,#12782,#12783,#12784,#12785,#12786,#12787,
#12788),.UNSPECIFIED.,.F.,.F.,(4,3,3,3,3,3,3,3,3,4),(-0.153261590805415,
-0.129427422483982,-0.117093626371441,-0.093122524304512,-0.077863059046492,
-0.0655799937729104,-0.0417579003169496,-0.0388648221790391,-0.0150894148558222,
0.),.UNSPECIFIED.);
#314=B_SPLINE_CURVE_WITH_KNOTS('',3,(#12791,#12792,#12793,#12794,#12795,
#12796,#12797,#12798,#12799,#12800,#12801,#12802,#12803,#12804,#12805,#12806,
#12807,#12808,#12809,#12810,#12811,#12812,#12813,#12814,#12815,#12816,#12817,
#12818),.UNSPECIFIED.,.F.,.F.,(4,3,3,3,3,3,3,3,3,4),(-0.153296867786173,
-0.129546774976449,-0.118009772088948,-0.0941871764575653,-0.08771862273971,
-0.0788646444725944,-0.0549216410880561,-0.0394902966566095,-0.0156128557692252,
0.),.UNSPECIFIED.);
#315=B_SPLINE_CURVE_WITH_KNOTS('',3,(#12835,#12836,#12837,#12838),
 .UNSPECIFIED.,.F.,.F.,(4,4),(-4.3123055228435,-0.796205213256333),
 .UNSPECIFIED.);
#316=B_SPLINE_CURVE_WITH_KNOTS('',3,(#12856,#12857,#12858,#12859),
 .UNSPECIFIED.,.F.,.F.,(4,4),(-0.594853877716395,-0.335767855111383),
 .UNSPECIFIED.);
#317=B_SPLINE_CURVE_WITH_KNOTS('',3,(#12860,#12861,#12862,#12863),
 .UNSPECIFIED.,.F.,.F.,(4,4),(-0.615688454110788,-0.00935595183171186),
 .UNSPECIFIED.);
#318=B_SPLINE_CURVE_WITH_KNOTS('',3,(#12884,#12885,#12886,#12887),
 .UNSPECIFIED.,.F.,.F.,(4,4),(0.806548880270408,4.31873271634551),
 .UNSPECIFIED.);
#319=B_SPLINE_CURVE_WITH_KNOTS('',3,(#12909,#12910,#12911,#12912),
 .UNSPECIFIED.,.F.,.F.,(4,4),(0.335767855111383,0.605460332260614),
 .UNSPECIFIED.);
#320=B_SPLINE_CURVE_WITH_KNOTS('',3,(#12915,#12916,#12917,#12918),
 .UNSPECIFIED.,.F.,.F.,(4,4),(8.8675541747208,12.379738010796),
 .UNSPECIFIED.);
#321=B_SPLINE_CURVE_WITH_KNOTS('',3,(#12921,#12922,#12923,#12924),
 .UNSPECIFIED.,.F.,.F.,(4,4),(12.5808265588057,12.8505190359549),
 .UNSPECIFIED.);
#322=B_SPLINE_CURVE_WITH_KNOTS('',3,(#12946,#12947,#12948,#12949),
 .UNSPECIFIED.,.F.,.F.,(4,4),(-12.3900816778099,-8.87398136822274),
 .UNSPECIFIED.);
#323=B_SPLINE_CURVE_WITH_KNOTS('',3,(#12983,#12984,#12985,#12986),
 .UNSPECIFIED.,.F.,.F.,(4,4),(0.00935595183171174,0.615688454110787),
 .UNSPECIFIED.);
#324=B_SPLINE_CURVE_WITH_KNOTS('',3,(#12987,#12988,#12989,#12990),
 .UNSPECIFIED.,.F.,.F.,(4,4),(-12.8505190359549,-12.5914330133498),
 .UNSPECIFIED.);
#325=B_SPLINE_CURVE_WITH_KNOTS('',3,(#12993,#12994,#12995,#12996,#12997,
#12998),.UNSPECIFIED.,.F.,.F.,(4,2,4),(-0.606830654194234,-0.303665168982051,
-0.00091389508118378),.UNSPECIFIED.);
#326=B_SPLINE_CURVE_WITH_KNOTS('',3,(#13000,#13001,#13002,#13003,#13004,
#13005,#13006,#13007,#13008,#13009,#13010,#13011,#13012,#13013,#13014,#13015,
#13016,#13017,#13018,#13019,#13020,#13021,#13022,#13023,#13024,#13025,#13026,
#13027),.UNSPECIFIED.,.F.,.F.,(4,3,3,3,3,3,3,3,3,4),(-0.152562937837783,
-0.12881903955137,-0.117160811640917,-0.0932181166800446,-0.0780374575565173,
-0.0653603882662585,-0.0415602279441365,-0.0389951227734853,-0.0152093108541457,
0.),.UNSPECIFIED.);
#327=B_SPLINE_CURVE_WITH_KNOTS('',3,(#13031,#13032,#13033,#13034,#13035,
#13036,#13037,#13038,#13039,#13040,#13041,#13042,#13043,#13044,#13045,#13046,
#13047,#13048,#13049,#13050,#13051,#13052,#13053,#13054,#13055,#13056,#13057,
#13058),.UNSPECIFIED.,.F.,.F.,(4,3,3,3,3,3,3,3,3,4),(-0.152573286042523,
-0.128801685906155,-0.115487540236632,-0.091707628219999,-0.0872268515824704,
-0.07838422198738,-0.0544695788315335,-0.0392121213631617,-0.0154211067806385,
0.),.UNSPECIFIED.);
#328=B_SPLINE_CURVE_WITH_KNOTS('',3,(#13059,#13060,#13061,#13062,#13063,
#13064),.UNSPECIFIED.,.F.,.F.,(4,2,4),(-0.606417229744719,-0.30366508312326,
-0.000500462001714608),.UNSPECIFIED.);
#329=B_SPLINE_CURVE_WITH_KNOTS('',3,(#13081,#13082,#13083,#13084),
 .UNSPECIFIED.,.F.,.F.,(4,4),(-8.7204856127415,-4.5128966022766),
 .UNSPECIFIED.);
#330=B_SPLINE_CURVE_WITH_KNOTS('',3,(#13105,#13106,#13107,#13108),
 .UNSPECIFIED.,.F.,.F.,(4,4),(4.51913891174751,8.72381854299666),
 .UNSPECIFIED.);
#331=B_SPLINE_CURVE_WITH_KNOTS('',3,(#13110,#13111,#13112,#13113),
 .UNSPECIFIED.,.F.,.F.,(4,4),(4.46246834806959,8.66714797931881),
 .UNSPECIFIED.);
#332=B_SPLINE_CURVE_WITH_KNOTS('',3,(#13134,#13135,#13136,#13137),
 .UNSPECIFIED.,.F.,.F.,(4,4),(-8.67339028878965,-4.46580127832475),
 .UNSPECIFIED.);
#333=B_SPLINE_CURVE_WITH_KNOTS('',3,(#13156,#13157,#13158,#13159,#13160,
#13161),.UNSPECIFIED.,.F.,.F.,(4,2,4),(-0.607391644691745,-0.303762155877002,
-0.00125172564267001),.UNSPECIFIED.);
#334=B_SPLINE_CURVE_WITH_KNOTS('',3,(#13162,#13163,#13164,#13165,#13166,
#13167,#13168,#13169,#13170,#13171,#13172,#13173,#13174,#13175,#13176,#13177,
#13178,#13179,#13180,#13181,#13182,#13183,#13184,#13185,#13186,#13187,#13188,
#13189),.UNSPECIFIED.,.F.,.F.,(4,3,3,3,3,3,3,3,3,4),(-0.152281539067936,
-0.12854821222061,-0.115190816126163,-0.0912758856104041,-0.0781043161616985,
-0.0652713841318381,-0.0414808619979686,-0.039045740680325,-0.0152551599791835,
0.),.UNSPECIFIED.);
#335=B_SPLINE_CURVE_WITH_KNOTS('',3,(#13191,#13192,#13193,#13194,#13195,
#13196,#13197,#13198,#13199,#13200,#13201,#13202,#13203,#13204,#13205,#13206,
#13207,#13208,#13209,#13210,#13211,#13212,#13213,#13214,#13215,#13216,#13217,
#13218),.UNSPECIFIED.,.F.,.F.,(4,3,3,3,3,3,3,3,3,4),(-0.152284734818265,
-0.128510300097745,-0.115243636037359,-0.0914764658269932,-0.0870316758632336,
-0.078197793898112,-0.0542955901223581,-0.0391042908842167,-0.0153462458625635,
0.),.UNSPECIFIED.);
#336=B_SPLINE_CURVE_WITH_KNOTS('',3,(#13219,#13220,#13221,#13222,#13223,
#13224),.UNSPECIFIED.,.F.,.F.,(4,2,4),(-0.606273164239037,-0.303762187833104,
-0.000133245189939568),.UNSPECIFIED.);
#337=B_SPLINE_CURVE_WITH_KNOTS('',3,(#13241,#13242,#13243,#13244),
 .UNSPECIFIED.,.F.,.F.,(4,4),(-12.1227852464729,-8.92068531110742),
 .UNSPECIFIED.);
#338=B_SPLINE_CURVE_WITH_KNOTS('',3,(#13285,#13286,#13287,#13288),
 .UNSPECIFIED.,.F.,.F.,(4,4),(-4.26560157995882,-1.06350164459338),
 .UNSPECIFIED.);
#339=B_SPLINE_CURVE_WITH_KNOTS('',3,(#13307,#13308,#13309,#13310,#13311,
#13312),.UNSPECIFIED.,.F.,.F.,(4,2,4),(-0.607545900263938,-0.303784727094449,
-0.00134539382494125),.UNSPECIFIED.);
#340=B_SPLINE_CURVE_WITH_KNOTS('',3,(#13314,#13315,#13316,#13317,#13318,
#13319,#13320,#13321,#13322,#13323,#13324,#13325,#13326,#13327,#13328,#13329,
#13330,#13331,#13332,#13333,#13334,#13335,#13336,#13337,#13338,#13339,#13340,
#13341),.UNSPECIFIED.,.F.,.F.,(4,3,3,3,3,3,3,3,3,4),(-0.152214473108837,
-0.128485298747135,-0.115164309990209,-0.0912534321321267,-0.0781163092888813,
-0.0652482412471129,-0.0414606388666645,-0.0390548598067502,-0.0152611452145655,
0.),.UNSPECIFIED.);
#341=B_SPLINE_CURVE_WITH_KNOTS('',3,(#13345,#13346,#13347,#13348,#13349,
#13350,#13351,#13352,#13353,#13354,#13355,#13356,#13357,#13358,#13359,#13360,
#13361,#13362,#13363,#13364,#13365,#13366,#13367,#13368,#13369,#13370,#13371,
#13372),.UNSPECIFIED.,.F.,.F.,(4,3,3,3,3,3,3,3,3,4),(-0.152216110966007,
-0.128438825687404,-0.115191384846861,-0.0914281188167518,-0.0869870566155827,
-0.0781642271790374,-0.0542662950786889,-0.0390848818783988,-0.0153309789665,
0.),.UNSPECIFIED.);
#342=B_SPLINE_CURVE_WITH_KNOTS('',3,(#13373,#13374,#13375,#13376,#13377,
#13378),.UNSPECIFIED.,.F.,.F.,(4,2,4),(-0.606227037063105,-0.303784766192107,
-2.65251918123988E-5),.UNSPECIFIED.);
#343=B_SPLINE_CURVE_WITH_KNOTS('',3,(#13396,#13397,#13398,#13399),
 .UNSPECIFIED.,.F.,.F.,(4,4),(0.0107208554739345,0.617725317592517),
 .UNSPECIFIED.);
#344=B_SPLINE_CURVE_WITH_KNOTS('',3,(#13400,#13401,#13402,#13403),
 .UNSPECIFIED.,.F.,.F.,(4,4),(-12.893479658151,-12.3228618033436),
 .UNSPECIFIED.);
#345=B_SPLINE_CURVE_WITH_KNOTS('',3,(#13426,#13427,#13428,#13429),
 .UNSPECIFIED.,.F.,.F.,(4,4),(12.3251818525939,12.893479658151),
 .UNSPECIFIED.);
#346=B_SPLINE_CURVE_WITH_KNOTS('',3,(#13433,#13434,#13435,#13436),
 .UNSPECIFIED.,.F.,.F.,(4,4),(0.292807233425235,0.861105038472338),
 .UNSPECIFIED.);
#347=B_SPLINE_CURVE_WITH_KNOTS('',3,(#13454,#13455,#13456,#13457),
 .UNSPECIFIED.,.F.,.F.,(4,4),(-0.863425087722636,-0.29280723291527),
 .UNSPECIFIED.);
#348=B_SPLINE_CURVE_WITH_KNOTS('',3,(#13458,#13459,#13460,#13461),
 .UNSPECIFIED.,.F.,.F.,(4,4),(-0.617725317592517,-0.0107208554739345),
 .UNSPECIFIED.);
#349=B_SPLINE_CURVE_WITH_KNOTS('',3,(#13545,#13546,#13547,#13548),
 .UNSPECIFIED.,.F.,.F.,(4,4),(0.00878563933291533,0.615688454110788),
 .UNSPECIFIED.);
#350=B_SPLINE_CURVE_WITH_KNOTS('',3,(#13573,#13574,#13575,#13576),
 .UNSPECIFIED.,.F.,.F.,(4,4),(-0.615688454110787,-0.00878563933291527),
 .UNSPECIFIED.);
#351=B_SPLINE_CURVE_WITH_KNOTS('',3,(#13662,#13663,#13664,#13665),
 .UNSPECIFIED.,.F.,.F.,(4,4),(-9.62771529167128E-17,0.617725317592517),
 .UNSPECIFIED.);
#352=B_SPLINE_CURVE_WITH_KNOTS('',3,(#13666,#13667,#13668,#13669),
 .UNSPECIFIED.,.F.,.F.,(4,4),(-0.617725317592517,-0.000337488966422091),
 .UNSPECIFIED.);
#353=B_SPLINE_CURVE_WITH_KNOTS('',3,(#13705,#13706,#13707,#13708,#13709),
 .UNSPECIFIED.,.F.,.F.,(4,1,4),(-12.893479658151,-5.71764434212835,-0.335767855111383),
 .UNSPECIFIED.);
#354=B_SPLINE_CURVE_WITH_KNOTS('',3,(#13710,#13711,#13712,#13713,#13714),
 .UNSPECIFIED.,.F.,.F.,(4,1,4),(0.335767855111383,5.71764434212835,12.893479658151),
 .UNSPECIFIED.);
#355=B_SPLINE_CURVE_WITH_KNOTS('',3,(#13739,#13740,#13741,#13742),
 .UNSPECIFIED.,.F.,.F.,(4,4),(-0.00171041937131743,0.615688454110788),
 .UNSPECIFIED.);
#356=B_SPLINE_CURVE_WITH_KNOTS('',3,(#13743,#13744,#13745,#13746),
 .UNSPECIFIED.,.F.,.F.,(4,4),(-0.615688454110788,-3.98826847727851E-7),
 .UNSPECIFIED.);
#357=B_SPLINE_CURVE_WITH_KNOTS('',3,(#13771,#13772,#13773,#13774),
 .UNSPECIFIED.,.F.,.F.,(4,4),(3.98826847219577E-7,0.615688454110787),
 .UNSPECIFIED.);
#358=B_SPLINE_CURVE_WITH_KNOTS('',3,(#13775,#13776,#13777,#13778),
 .UNSPECIFIED.,.F.,.F.,(4,4),(-0.615688454110787,0.0017104193713176),
 .UNSPECIFIED.);
#359=B_SPLINE_CURVE_WITH_KNOTS('',3,(#13804,#13805,#13806,#13807,#13808),
 .UNSPECIFIED.,.F.,.F.,(4,1,4),(-12.8505190359549,-7.4686425489379,-0.29280723291527),
 .UNSPECIFIED.);
#360=B_SPLINE_CURVE_WITH_KNOTS('',3,(#13809,#13810,#13811,#13812,#13813),
 .UNSPECIFIED.,.F.,.F.,(4,1,4),(0.292807233425236,7.4686425489379,12.8505190359549),
 .UNSPECIFIED.);
#361=B_SPLINE_CURVE_WITH_KNOTS('',3,(#13834,#13835,#13836,#13837),
 .UNSPECIFIED.,.F.,.F.,(4,4),(0.000337488966421928,0.617725317592517),
 .UNSPECIFIED.);
#362=B_SPLINE_CURVE_WITH_KNOTS('',3,(#13838,#13839,#13840,#13841),
 .UNSPECIFIED.,.F.,.F.,(4,4),(-0.617725317592517,8.06646416329215E-17),
 .UNSPECIFIED.);
#363=B_SPLINE_CURVE_WITH_KNOTS('',3,(#13975,#13976,#13977,#13978,#13979),
 .UNSPECIFIED.,.F.,.F.,(4,1,4),(-0.118017359897249,-0.0505788685273923,
0.),.UNSPECIFIED.);
#364=B_SPLINE_CURVE_WITH_KNOTS('',3,(#13982,#13983,#13984,#13985,#13986),
 .UNSPECIFIED.,.F.,.F.,(4,1,4),(0.,0.0505788685273923,0.118017359897249),
 .UNSPECIFIED.);
#365=B_SPLINE_CURVE_WITH_KNOTS('',3,(#14021,#14022,#14023,#14024,#14025),
 .UNSPECIFIED.,.F.,.F.,(4,1,4),(-0.118017359898262,-0.0505788685278266,
0.),.UNSPECIFIED.);
#366=B_SPLINE_CURVE_WITH_KNOTS('',3,(#14026,#14027,#14028,#14029,#14030),
 .UNSPECIFIED.,.F.,.F.,(4,1,4),(0.,0.0505788685278266,0.118017359898262),
 .UNSPECIFIED.);
#367=B_SPLINE_CURVE_WITH_KNOTS('',3,(#14059,#14060,#14061,#14062,#14063),
 .UNSPECIFIED.,.F.,.F.,(4,1,4),(-12.2100728150593,-5.23288834931112,0.),
 .UNSPECIFIED.);
#368=B_SPLINE_CURVE_WITH_KNOTS('',3,(#14064,#14065,#14066,#14067,#14068),
 .UNSPECIFIED.,.F.,.F.,(4,1,4),(0.,5.23288834931112,12.2100728150593),
 .UNSPECIFIED.);
#369=B_SPLINE_CURVE_WITH_KNOTS('',3,(#14097,#14098,#14099,#14100,#14101),
 .UNSPECIFIED.,.F.,.F.,(4,1,4),(-0.108129892237767,-0.0463413823988794,
-1.97133828064127E-11),.UNSPECIFIED.);
#370=B_SPLINE_CURVE_WITH_KNOTS('',3,(#14102,#14103,#14104,#14105,#14106),
 .UNSPECIFIED.,.F.,.F.,(4,1,4),(1.97133828064127E-11,0.0463413823988794,
0.108129892237767),.UNSPECIFIED.);
#371=B_SPLINE_CURVE_WITH_KNOTS('',3,(#14141,#14142,#14143,#14144,#14145),
 .UNSPECIFIED.,.F.,.F.,(4,1,4),(-0.108129892206815,-0.0463413823743492,
0.),.UNSPECIFIED.);
#372=B_SPLINE_CURVE_WITH_KNOTS('',3,(#14146,#14147,#14148,#14149,#14150),
 .UNSPECIFIED.,.F.,.F.,(4,1,4),(0.,0.0463413823743492,0.108129892206815),
 .UNSPECIFIED.);
#373=B_SPLINE_CURVE_WITH_KNOTS('',3,(#14176,#14177,#14178,#14179,#14180),
 .UNSPECIFIED.,.F.,.F.,(4,1,4),(-12.2100734167563,-6.97718480957529,-6.51086303075479E-13),
 .UNSPECIFIED.);
#374=B_SPLINE_CURVE_WITH_KNOTS('',3,(#14181,#14182,#14183,#14184,#14185),
 .UNSPECIFIED.,.F.,.F.,(4,1,4),(6.51086303075479E-13,6.97718480957529,12.2100734167563),
 .UNSPECIFIED.);
#375=B_SPLINE_CURVE_WITH_KNOTS('',3,(#14188,#14189,#14190,#14191),
 .UNSPECIFIED.,.F.,.F.,(4,4),(0.000181689894813921,0.124708996845866),
 .UNSPECIFIED.);
#376=B_SPLINE_CURVE_WITH_KNOTS('',3,(#14194,#14195,#14196,#14197),
 .UNSPECIFIED.,.F.,.F.,(4,4),(-0.124708996851356,-0.000181689894814102),
 .UNSPECIFIED.);
#377=B_SPLINE_CURVE_WITH_KNOTS('',3,(#14219,#14220,#14221,#14222),
 .UNSPECIFIED.,.F.,.F.,(4,4),(-0.124624122980966,-1.27068494615301E-16),
 .UNSPECIFIED.);
#378=B_SPLINE_CURVE_WITH_KNOTS('',3,(#14223,#14224,#14225,#14226,#14227,
#14228,#14229,#14230,#14231,#14232,#14233,#14234,#14235,#14236,#14237,#14238,
#14239,#14240,#14241,#14242,#14243,#14244,#14245,#14246,#14247,#14248,#14249,
#14250),.UNSPECIFIED.,.F.,.F.,(4,3,3,3,3,3,3,3,3,4),(0.,0.0322747504276753,
0.0586406101183928,0.090870813631105,0.0996503787243826,0.117132790114159,
0.149546322800321,0.175583390425035,0.207787925145658,0.232457773984835),
 .UNSPECIFIED.);
#379=B_SPLINE_CURVE_WITH_KNOTS('',3,(#14268,#14269,#14270,#14271),
 .UNSPECIFIED.,.F.,.F.,(4,4),(6.28713621962651E-9,0.124025126494243),
 .UNSPECIFIED.);
#380=B_SPLINE_CURVE_WITH_KNOTS('',3,(#14272,#14273,#14274,#14275),
 .UNSPECIFIED.,.F.,.F.,(4,4),(0.0116899650356219,0.986620910196183),
 .UNSPECIFIED.);
#381=B_SPLINE_CURVE_WITH_KNOTS('',3,(#14301,#14302,#14303,#14304),
 .UNSPECIFIED.,.F.,.F.,(4,4),(-0.12358375933533,0.000944809985246663),
 .UNSPECIFIED.);
#382=B_SPLINE_CURVE_WITH_KNOTS('',3,(#14305,#14306,#14307,#14308,#14309,
#14310,#14311,#14312,#14313,#14314,#14315,#14316,#14317,#14318,#14319,#14320,
#14321,#14322,#14323,#14324,#14325,#14326,#14327,#14328,#14329,#14330,#14331,
#14332,#14333,#14334,#14335,#14336,#14337,#14338),.UNSPECIFIED.,.F.,.F.,
(4,3,3,3,3,3,3,3,3,3,3,4),(0.,0.0322568536241053,0.0586526138523664,0.0909514856947606,
0.108742407475907,0.117151788463556,0.149394351344039,0.175600627102286,
0.181167420983902,0.214570374458228,0.246736309066329,0.253563811229603),
 .UNSPECIFIED.);
#383=B_SPLINE_CURVE_WITH_KNOTS('',3,(#14342,#14343,#14344,#14345),
 .UNSPECIFIED.,.F.,.F.,(4,4),(-0.000944809985246617,0.123583759335329),
 .UNSPECIFIED.);
#384=B_SPLINE_CURVE_WITH_KNOTS('',3,(#14368,#14369,#14370,#14371,#14372,
#14373,#14374,#14375,#14376,#14377,#14378,#14379,#14380,#14381,#14382,#14383,
#14384,#14385,#14386,#14387,#14388,#14389,#14390,#14391,#14392,#14393,#14394,
#14395),.UNSPECIFIED.,.F.,.F.,(4,3,3,3,3,3,3,3,3,4),(0.,0.0322765438584903,
0.0586513922310012,0.0908809480268686,0.099655003871439,0.117150238497558,
0.149564657711791,0.175599638586681,0.20780211537115,0.232458396023953),
 .UNSPECIFIED.);
#385=B_SPLINE_CURVE_WITH_KNOTS('',3,(#14396,#14397,#14398,#14399),
 .UNSPECIFIED.,.F.,.F.,(4,4),(3.30031141304588E-16,0.124624122970512),
 .UNSPECIFIED.);
#386=B_SPLINE_CURVE_WITH_KNOTS('',3,(#14425,#14426,#14427,#14428),
 .UNSPECIFIED.,.F.,.F.,(4,4),(-0.12402512649425,-6.28713634712869E-9),
 .UNSPECIFIED.);
#387=B_SPLINE_CURVE_WITH_KNOTS('',3,(#14429,#14430,#14431,#14432,#14433,
#14434,#14435,#14436,#14437,#14438,#14439,#14440,#14441,#14442,#14443,#14444,
#14445,#14446,#14447,#14448,#14449,#14450,#14451,#14452,#14453,#14454,#14455,
#14456,#14457,#14458,#14459,#14460,#14461,#14462),.UNSPECIFIED.,.F.,.F.,
(4,3,3,3,3,3,3,3,3,3,3,4),(0.,0.0322666769662355,0.0587055335553437,0.0910029078093924,
0.108768157423115,0.117242626226166,0.149488313345073,0.175692943342501,
0.181189289804584,0.214619150478997,0.24677571115805,0.253566775541772),
 .UNSPECIFIED.);
#388=B_SPLINE_CURVE_WITH_KNOTS('',3,(#14464,#14465,#14466,#14467),
 .UNSPECIFIED.,.F.,.F.,(4,4),(0.0133790898038168,0.988310034964378),
 .UNSPECIFIED.);
#389=B_SPLINE_CURVE_WITH_KNOTS('',3,(#14490,#14491,#14492,#14493,#14494,
#14495,#14496,#14497,#14498,#14499),.UNSPECIFIED.,.F.,.F.,(4,3,3,4),(-4.09202352044852,
-3.99057144343763,-2.99292858257822,-2.07317267331971),.UNSPECIFIED.);
#390=B_SPLINE_CURVE_WITH_KNOTS('',3,(#14502,#14503,#14504,#14505,#14506,
#14507,#14508),.UNSPECIFIED.,.F.,.F.,(4,3,4),(0.,0.998042281124014,1.12274180646116),
 .UNSPECIFIED.);
#391=B_SPLINE_CURVE_WITH_KNOTS('',3,(#14513,#14514,#14515,#14516,#14517,
#14518,#14519,#14520,#14521,#14522,#14523,#14524,#14525,#14526,#14527,#14528,
#14529,#14530,#14531,#14532,#14533,#14534),.UNSPECIFIED.,.F.,.F.,(4,3,3,
3,3,3,3,4),(-10.3752088276281,-9.97642860859406,-8.97878574773466,-7.98114288687525,
-6.98350002601584,-5.98585716515644,-4.98821430429703,-4.09202352044852),
 .UNSPECIFIED.);
#392=B_SPLINE_CURVE_WITH_KNOTS('',3,(#14535,#14536,#14537,#14538,#14539,
#14540,#14541,#14542,#14543,#14544,#14545,#14546,#14547,#14548,#14549,#14550,
#14551,#14552,#14553,#14554,#14555,#14556),.UNSPECIFIED.,.F.,.F.,(4,3,3,
3,3,3,3,4),(1.12274180646116,1.99608456224804,2.99412684337208,3.99216912449611,
4.99021140562014,5.98825368674417,6.98629596786821,7.40592711364074),
 .UNSPECIFIED.);
#393=B_SPLINE_CURVE_WITH_KNOTS('',3,(#14561,#14562,#14563,#14564,#14565,
#14566,#14567,#14568,#14569,#14570,#14571,#14572,#14573,#14574,#14575,#14576,
#14577,#14578,#14579,#14580,#14581,#14582),.UNSPECIFIED.,.F.,.F.,(4,3,3,
3,3,3,3,4),(-16.6583941348077,-15.9622857737505,-14.9646429128911,-13.9670000520317,
-12.9693571911723,-11.9717143303129,-10.9740714694535,-10.3752088276281),
 .UNSPECIFIED.);
#394=B_SPLINE_CURVE_WITH_KNOTS('',3,(#14583,#14584,#14585,#14586,#14587,
#14588,#14589,#14590,#14591,#14592,#14593,#14594,#14595,#14596,#14597,#14598,
#14599,#14600,#14601,#14602,#14603,#14604),.UNSPECIFIED.,.F.,.F.,(4,3,3,
3,3,3,3,4),(7.40592711364074,7.98433824899223,8.98238053011626,9.98042281124028,
10.9784650923643,11.9765073734883,12.9745496546124,13.6891124208203),
 .UNSPECIFIED.);
#395=B_SPLINE_CURVE_WITH_KNOTS('',3,(#14609,#14610,#14611,#14612,#14613,
#14614,#14615,#14616,#14617,#14618,#14619,#14620,#14621,#14622,#14623,#14624,
#14625,#14626,#14627,#14628,#14629,#14630),.UNSPECIFIED.,.F.,.F.,(4,3,3,
3,3,3,3,4),(-22.9415794419873,-21.9481429389069,-20.9505000780475,-19.9528572171881,
-18.9552143563287,-17.9575714954693,-16.9599286346099,-16.6583941348077),
 .UNSPECIFIED.);
#396=B_SPLINE_CURVE_WITH_KNOTS('',3,(#14631,#14632,#14633,#14634,#14635,
#14636,#14637,#14638,#14639,#14640,#14641,#14642,#14643,#14644,#14645,#14646,
#14647,#14648,#14649,#14650,#14651,#14652,#14653,#14654,#14655),
 .UNSPECIFIED.,.F.,.F.,(4,3,3,3,3,3,3,3,4),(13.6891124208203,13.9725919357364,
14.9706342168604,15.9686764979844,16.9667187791085,17.9647610602325,18.9628033413565,
19.9608456224805,19.9722977279999),.UNSPECIFIED.);
#397=B_SPLINE_CURVE_WITH_KNOTS('',3,(#14660,#14661,#14662,#14663,#14664,
#14665,#14666,#14667,#14668,#14669,#14670,#14671,#14672,#14673,#14674,#14675,
#14676,#14677,#14678,#14679,#14680,#14681),.UNSPECIFIED.,.F.,.F.,(4,3,3,
3,3,3,3,4),(-29.2247647491669,-28.9316429649228,-27.9340001040634,-26.936357243204,
-25.9387143823446,-24.9410715214852,-23.9434286606257,-22.9415794419873),
 .UNSPECIFIED.);
#398=B_SPLINE_CURVE_WITH_KNOTS('',3,(#14682,#14683,#14684,#14685,#14686,
#14687,#14688,#14689,#14690,#14691,#14692,#14693,#14694,#14695,#14696,#14697,
#14698,#14699,#14700,#14701,#14702,#14703),.UNSPECIFIED.,.F.,.F.,(4,3,3,
3,3,3,3,4),(19.9722977279999,20.9588879036046,21.9569301847286,22.9549724658526,
23.9530147469767,24.9510570281007,25.9490993092247,26.2554830351795),
 .UNSPECIFIED.);
#399=B_SPLINE_CURVE_WITH_KNOTS('',3,(#14708,#14709,#14710,#14711,#14712,
#14713,#14714,#14715,#14716,#14717,#14718,#14719,#14720,#14721,#14722,#14723,
#14724,#14725,#14726,#14727,#14728,#14729),.UNSPECIFIED.,.F.,.F.,(4,3,3,
3,3,3,3,4),(-35.5079500563465,-34.9175001300792,-33.9198572692198,-32.9222144083604,
-31.924571547501,-30.9269286866416,-29.9292858257822,-29.2247647491669),
 .UNSPECIFIED.);
#400=B_SPLINE_CURVE_WITH_KNOTS('',3,(#14730,#14731,#14732,#14733,#14734,
#14735,#14736,#14737,#14738,#14739,#14740,#14741,#14742,#14743,#14744,#14745,
#14746,#14747,#14748,#14749,#14750,#14751),.UNSPECIFIED.,.F.,.F.,(4,3,3,
3,3,3,3,4),(26.2554830351795,26.9471415903487,27.9451838714728,28.9432261525968,
29.9412684337208,30.9393107148448,31.9373529959689,32.5386683423591),
 .UNSPECIFIED.);
#401=B_SPLINE_CURVE_WITH_KNOTS('',3,(#14756,#14757,#14758,#14759,#14760,
#14761,#14762,#14763,#14764,#14765,#14766,#14767,#14768,#14769,#14770,#14771,
#14772,#14773,#14774,#14775,#14776,#14777),.UNSPECIFIED.,.F.,.F.,(4,3,3,
3,3,3,3,4),(-41.791135363526,-40.9033572952357,-39.9057144343762,-38.9080715735168,
-37.9104287126574,-36.912785851798,-35.9151429909386,-35.5079500563465),
 .UNSPECIFIED.);
#402=B_SPLINE_CURVE_WITH_KNOTS('',3,(#14778,#14779,#14780,#14781,#14782,
#14783,#14784,#14785,#14786,#14787,#14788,#14789,#14790,#14791,#14792,#14793,
#14794,#14795,#14796,#14797,#14798,#14799),.UNSPECIFIED.,.F.,.F.,(4,3,3,
3,3,3,3,4),(32.5386683423591,32.9353952770929,33.9334375582169,34.931479839341,
35.929522120465,36.927564401589,37.9256066827131,38.8218536495387),
 .UNSPECIFIED.);
#403=B_SPLINE_CURVE_WITH_KNOTS('',3,(#14804,#14805,#14806,#14807,#14808,
#14809,#14810,#14811,#14812,#14813,#14814,#14815,#14816,#14817,#14818,#14819,
#14820,#14821,#14822,#14823,#14824,#14825,#14826,#14827,#14828),
 .UNSPECIFIED.,.F.,.F.,(4,3,3,3,3,3,3,3,4),(-48.0743206707056,-47.8868573212515,
-46.8892144603921,-45.8915715995327,-44.8939287386733,-43.8962858778139,
-42.8986430169545,-41.9010001560951,-41.791135363526),.UNSPECIFIED.);
#404=B_SPLINE_CURVE_WITH_KNOTS('',3,(#14829,#14830,#14831,#14832,#14833,
#14834,#14835,#14836,#14837,#14838,#14839,#14840,#14841,#14842,#14843,#14844,
#14845,#14846,#14847,#14848,#14849,#14850,#14851,#14852,#14853),
 .UNSPECIFIED.,.F.,.F.,(4,3,3,3,3,3,3,3,4),(38.8218536495387,38.9236489638371,
39.9216912449611,40.9197335260851,41.9177758072091,42.9158180883332,43.9138603694572,
44.9119026505812,45.1050389567183),.UNSPECIFIED.);
#405=B_SPLINE_CURVE_WITH_KNOTS('',3,(#14858,#14859,#14860,#14861,#14862,
#14863,#14864,#14865,#14866,#14867,#14868,#14869,#14870,#14871,#14872,#14873,
#14874,#14875,#14876,#14877,#14878,#14879),.UNSPECIFIED.,.F.,.F.,(4,3,3,
3,3,3,3,4),(-54.3575059778852,-53.8727144864079,-52.8750716255485,-51.8774287646891,
-50.8797859038297,-49.8821430429703,-48.8845001821109,-48.0743206707056),
 .UNSPECIFIED.);
#406=B_SPLINE_CURVE_WITH_KNOTS('',3,(#14880,#14881,#14882,#14883,#14884,
#14885,#14886,#14887,#14888,#14889,#14890,#14891,#14892,#14893,#14894,#14895,
#14896,#14897,#14898,#14899,#14900,#14901),.UNSPECIFIED.,.F.,.F.,(4,3,3,
3,3,3,3,4),(45.1050389567183,45.9099449317052,46.9079872128293,47.9060294939533,
48.9040717750773,49.9021140562014,50.9001563373254,51.3882242638979),
 .UNSPECIFIED.);
#407=B_SPLINE_CURVE_WITH_KNOTS('',3,(#14906,#14907,#14908,#14909,#14910,
#14911,#14912,#14913,#14914,#14915,#14916,#14917,#14918,#14919,#14920,#14921,
#14922,#14923,#14924,#14925,#14926,#14927),.UNSPECIFIED.,.F.,.F.,(4,3,3,
3,3,3,3,4),(-60.6406912850648,-59.8585716515644,-58.860928790705,-57.8632859298455,
-56.8656430689861,-55.8680002081267,-54.8703573472673,-54.3575059778852),
 .UNSPECIFIED.);
#408=B_SPLINE_CURVE_WITH_KNOTS('',3,(#14928,#14929,#14930,#14931,#14932,
#14933,#14934,#14935,#14936,#14937,#14938,#14939,#14940,#14941,#14942,#14943,
#14944,#14945,#14946,#14947,#14948,#14949),.UNSPECIFIED.,.F.,.F.,(4,3,3,
3,3,3,3,4),(51.3882242638979,51.8981986184494,52.8962408995734,53.8942831806975,
54.8923254618215,55.8903677429455,56.8884100240695,57.6714095710775),
 .UNSPECIFIED.);
#409=B_SPLINE_CURVE_WITH_KNOTS('',3,(#14954,#14955,#14956,#14957,#14958,
#14959,#14960,#14961,#14962,#14963,#14964,#14965,#14966,#14967,#14968,#14969,
#14970,#14971,#14972,#14973,#14974,#14975,#14976,#14977,#14978),
 .UNSPECIFIED.,.F.,.F.,(4,3,3,3,3,3,3,3,4),(-66.9238765922444,-66.8420716775802,
-65.8444288167208,-64.8467859558614,-63.849143095002,-62.8515002341426,
-61.8538573732832,-60.8562145124238,-60.6406912850648),.UNSPECIFIED.);
#410=B_SPLINE_CURVE_WITH_KNOTS('',3,(#14979,#14980,#14981,#14982,#14983,
#14984,#14985,#14986,#14987,#14988,#14989,#14990,#14991,#14992,#14993,#14994,
#14995,#14996,#14997,#14998,#14999,#15000,#15001,#15002,#15003),
 .UNSPECIFIED.,.F.,.F.,(4,3,3,3,3,3,3,3,4),(57.6714095710775,57.8864523051936,
58.8844945863176,59.8825368674416,60.8805791485657,61.8786214296897,62.8766637108137,
63.8747059919378,63.9545948782571),.UNSPECIFIED.);
#411=B_SPLINE_CURVE_WITH_KNOTS('',3,(#15008,#15009,#15010,#15011,#15012,
#15013,#15014,#15015,#15016,#15017,#15018,#15019,#15020,#15021,#15022,#15023,
#15024,#15025,#15026,#15027,#15028,#15029),.UNSPECIFIED.,.F.,.F.,(4,3,3,
3,3,3,3,4),(-73.207061899424,-72.8279288427366,-71.8302859818773,-70.8326431210178,
-69.8350002601584,-68.837357399299,-67.8397145384396,-66.9238765922444),
 .UNSPECIFIED.);
#412=B_SPLINE_CURVE_WITH_KNOTS('',3,(#15030,#15031,#15032,#15033,#15034,
#15035,#15036,#15037,#15038,#15039,#15040,#15041,#15042,#15043,#15044,#15045,
#15046,#15047,#15048,#15049,#15050,#15051),.UNSPECIFIED.,.F.,.F.,(4,3,3,
3,3,3,3,4),(63.9545948782571,64.8727482730618,65.8707905541858,66.8688328353098,
67.8668751164338,68.8649173975579,69.8629596786819,70.2377801854366),
 .UNSPECIFIED.);
#413=B_SPLINE_CURVE_WITH_KNOTS('',3,(#15056,#15057,#15058,#15059,#15060,
#15061,#15062,#15063,#15064,#15065,#15066,#15067,#15068,#15069,#15070,#15071,
#15072,#15073,#15074,#15075,#15076,#15077),.UNSPECIFIED.,.F.,.F.,(4,3,3,
3,3,3,3,4),(-79.4902472066036,-78.8137860078931,-77.8161431470337,-76.8185002861743,
-75.8208574253149,-74.8232145644555,-73.825571703596,-73.207061899424),
 .UNSPECIFIED.);
#414=B_SPLINE_CURVE_WITH_KNOTS('',3,(#15078,#15079,#15080,#15081,#15082,
#15083,#15084,#15085,#15086,#15087,#15088,#15089,#15090,#15091,#15092,#15093,
#15094,#15095,#15096,#15097,#15098,#15099),.UNSPECIFIED.,.F.,.F.,(4,3,3,
3,3,3,3,4),(70.2377801854366,70.8610019598059,71.85904424093,72.857086522054,
73.855128803178,74.853171084302,75.8512133654261,76.5209654926162),
 .UNSPECIFIED.);
#415=B_SPLINE_CURVE_WITH_KNOTS('',3,(#15104,#15105,#15106,#15107,#15108,
#15109,#15110,#15111,#15112,#15113,#15114,#15115,#15116,#15117,#15118,#15119,
#15120,#15121,#15122,#15123,#15124,#15125),.UNSPECIFIED.,.F.,.F.,(4,3,3,
3,3,3,3,4),(-85.7734325137832,-84.7996431730495,-83.8020003121901,-82.8043574513307,
-81.8067145904713,-80.8090717296119,-79.8114288687525,-79.4902472066036),
 .UNSPECIFIED.);
#416=B_SPLINE_CURVE_WITH_KNOTS('',3,(#15126,#15127,#15128,#15129,#15130,
#15131,#15132,#15133,#15134,#15135,#15136,#15137,#15138,#15139,#15140,#15141,
#15142,#15143,#15144,#15145,#15146,#15147),.UNSPECIFIED.,.F.,.F.,(4,3,3,
3,3,3,3,4),(76.5209654926162,76.8492556465501,77.8472979276741,78.8453402087982,
79.8433824899222,80.8414247710462,81.8394670521702,82.8041507997958),
 .UNSPECIFIED.);
#417=B_SPLINE_CURVE_WITH_KNOTS('',3,(#15152,#15153,#15154,#15155,#15156,
#15157,#15158,#15159,#15160,#15161,#15162,#15163,#15164,#15165,#15166,#15167,
#15168,#15169,#15170,#15171,#15172,#15173,#15174,#15175,#15176),
 .UNSPECIFIED.,.F.,.F.,(4,3,3,3,3,3,3,3,4),(-92.0566178209628,-91.7831431990654,
-90.7855003382059,-89.7878574773465,-88.7902146164871,-87.7925717556277,
-86.7949288947683,-85.7972860339089,-85.7734325137832),.UNSPECIFIED.);
#418=B_SPLINE_CURVE_WITH_KNOTS('',3,(#15177,#15178,#15179,#15180,#15181,
#15182,#15183,#15184,#15185,#15186,#15187,#15188,#15189,#15190,#15191,#15192,
#15193,#15194,#15195,#15196,#15197,#15198,#15199,#15200,#15201),
 .UNSPECIFIED.,.F.,.F.,(4,3,3,3,3,3,3,3,4),(82.8041507997958,82.8375093332942,
83.8355516144183,84.8335938955423,85.8316361766664,86.8296784577904,87.8277207389144,
88.8257630200384,89.0873361069754),.UNSPECIFIED.);
#419=B_SPLINE_CURVE_WITH_KNOTS('',3,(#15206,#15207,#15208,#15209,#15210,
#15211,#15212,#15213,#15214,#15215,#15216,#15217,#15218,#15219,#15220,#15221,
#15222,#15223,#15224,#15225,#15226,#15227),.UNSPECIFIED.,.F.,.F.,(4,3,3,
3,3,3,3,4),(-98.3398031281424,-97.7690003642218,-96.7713575033624,-95.773714642503,
-94.7760717816436,-93.7784289207842,-92.7807860599248,-92.0566178209628),
 .UNSPECIFIED.);
#420=B_SPLINE_CURVE_WITH_KNOTS('',3,(#15228,#15229,#15230,#15231,#15232,
#15233,#15234,#15235,#15236,#15237,#15238,#15239,#15240,#15241,#15242,#15243,
#15244,#15245,#15246,#15247,#15248,#15249),.UNSPECIFIED.,.F.,.F.,(4,3,3,
3,3,3,3,4),(89.0873361069754,89.8238053011624,90.8218475822865,91.8198898634105,
92.8179321445345,93.8159744256585,94.8140167067826,95.370521414155),
 .UNSPECIFIED.);
#421=B_SPLINE_CURVE_WITH_KNOTS('',3,(#15254,#15255,#15256,#15257,#15258,
#15259,#15260,#15261,#15262,#15263,#15264,#15265,#15266,#15267,#15268,#15269,
#15270,#15271,#15272,#15273,#15274,#15275),.UNSPECIFIED.,.F.,.F.,(4,3,3,
3,3,3,3,4),(-104.622988435322,-103.754857529378,-102.757214668519,-101.759571807659,
-100.7619289468,-99.7642860859406,-98.7666432250812,-98.3398031281424),
 .UNSPECIFIED.);
#422=B_SPLINE_CURVE_WITH_KNOTS('',3,(#15276,#15277,#15278,#15279,#15280,
#15281,#15282,#15283,#15284,#15285,#15286,#15287,#15288,#15289,#15290,#15291,
#15292,#15293,#15294,#15295,#15296,#15297),.UNSPECIFIED.,.F.,.F.,(4,3,3,
3,3,3,3,4),(95.370521414155,95.8120589879066,96.8101012690306,97.8081435501546,
98.8061858312787,99.8042281124027,100.802270393527,101.653706721335),
 .UNSPECIFIED.);
#423=B_SPLINE_CURVE_WITH_KNOTS('',3,(#15302,#15303,#15304,#15305,#15306,
#15307,#15308,#15309,#15310,#15311,#15312,#15313,#15314,#15315,#15316,#15317,
#15318,#15319,#15320,#15321,#15322,#15323,#15324,#15325,#15326),
 .UNSPECIFIED.,.F.,.F.,(4,3,3,3,3,3,3,3,4),(-110.906173742502,-110.738357555394,
-109.740714694535,-108.743071833675,-107.745428972816,-106.747786111956,
-105.750143251097,-104.752500390238,-104.622988435322),.UNSPECIFIED.);
#424=B_SPLINE_CURVE_WITH_KNOTS('',3,(#15327,#15328,#15329,#15330,#15331,
#15332,#15333,#15334,#15335,#15336,#15337,#15338,#15339,#15340,#15341,#15342,
#15343,#15344,#15345,#15346,#15347,#15348,#15349,#15350,#15351),
 .UNSPECIFIED.,.F.,.F.,(4,3,3,3,3,3,3,3,4),(101.653706721335,101.800312674651,
102.798354955775,103.796397236899,104.794439518023,105.792481799147,106.790524080271,
107.788566361395,107.936892028514),.UNSPECIFIED.);
#425=B_SPLINE_CURVE_WITH_KNOTS('',3,(#15356,#15357,#15358,#15359,#15360,
#15361,#15362,#15363,#15364,#15365,#15366,#15367,#15368,#15369,#15370,#15371,
#15372,#15373,#15374,#15375,#15376,#15377),.UNSPECIFIED.,.F.,.F.,(4,3,3,
3,3,3,3,4),(-117.189359049681,-116.724214720551,-115.726571859691,-114.728928998832,
-113.731286137972,-112.733643277113,-111.736000416253,-110.906173742502),
 .UNSPECIFIED.);
#426=B_SPLINE_CURVE_WITH_KNOTS('',3,(#15378,#15379,#15380,#15381,#15382,
#15383,#15384,#15385,#15386,#15387,#15388,#15389,#15390,#15391,#15392,#15393,
#15394,#15395,#15396,#15397,#15398,#15399),.UNSPECIFIED.,.F.,.F.,(4,3,3,
3,3,3,3,4),(107.936892028514,108.786608642519,109.784650923643,110.782693204767,
111.780735485891,112.778777767015,113.776820048139,114.220077335694),
 .UNSPECIFIED.);
#427=B_SPLINE_CURVE_WITH_KNOTS('',3,(#15404,#15405,#15406,#15407,#15408,
#15409,#15410,#15411,#15412,#15413,#15414,#15415,#15416,#15417,#15418,#15419,
#15420,#15421,#15422,#15423,#15424,#15425),.UNSPECIFIED.,.F.,.F.,(4,3,3,
3,3,3,3,4),(-123.472544356861,-122.710071885707,-121.712429024848,-120.714786163988,
-119.717143303129,-118.719500442269,-117.72185758141,-117.189359049681),
 .UNSPECIFIED.);
#428=B_SPLINE_CURVE_WITH_KNOTS('',3,(#15426,#15427,#15428,#15429,#15430,
#15431,#15432,#15433,#15434,#15435,#15436,#15437,#15438,#15439,#15440,#15441,
#15442,#15443,#15444,#15445,#15446,#15447),.UNSPECIFIED.,.F.,.F.,(4,3,3,
3,3,3,3,4),(114.220077335694,114.774862329263,115.772904610387,116.770946891511,
117.768989172635,118.767031453759,119.765073734883,120.503262642873),
 .UNSPECIFIED.);
#429=B_SPLINE_CURVE_WITH_KNOTS('',3,(#15452,#15453,#15454,#15455,#15456,
#15457,#15458,#15459,#15460,#15461,#15462,#15463,#15464,#15465,#15466,#15467,
#15468,#15469,#15470,#15471,#15472,#15473,#15474,#15475,#15476),
 .UNSPECIFIED.,.F.,.F.,(4,3,3,3,3,3,3,3,4),(-129.75572966404,-129.693571911723,
-128.695929050863,-127.698286190004,-126.700643329145,-125.703000468285,
-124.705357607426,-123.707714746566,-123.472544356861),.UNSPECIFIED.);
#430=B_SPLINE_CURVE_WITH_KNOTS('',3,(#15477,#15478,#15479,#15480,#15481,
#15482,#15483,#15484,#15485,#15486,#15487,#15488,#15489,#15490,#15491,#15492,
#15493,#15494,#15495,#15496,#15497,#15498,#15499,#15500,#15501),
 .UNSPECIFIED.,.F.,.F.,(4,3,3,3,3,3,3,3,4),(120.503262642873,120.763116016007,
121.761158297131,122.759200578255,123.757242859379,124.755285140503,125.753327421627,
126.751369702751,126.786447950053),.UNSPECIFIED.);
#431=B_SPLINE_CURVE_WITH_KNOTS('',3,(#15506,#15507,#15508,#15509,#15510,
#15511,#15512,#15513,#15514,#15515,#15516,#15517,#15518,#15519,#15520,#15521,
#15522,#15523,#15524,#15525,#15526,#15527),.UNSPECIFIED.,.F.,.F.,(4,3,3,
3,3,3,3,4),(-136.03891497122,-135.679429076879,-134.68178621602,-133.68414335516,
-132.686500494301,-131.688857633442,-130.691214772582,-129.75572966404),
 .UNSPECIFIED.);
#432=B_SPLINE_CURVE_WITH_KNOTS('',3,(#15528,#15529,#15530,#15531,#15532,
#15533,#15534,#15535,#15536,#15537,#15538,#15539,#15540,#15541,#15542,#15543,
#15544,#15545,#15546,#15547,#15548,#15549),.UNSPECIFIED.,.F.,.F.,(4,3,3,
3,3,3,3,4),(126.786447950053,127.749411983875,128.747454265,129.745496546124,
130.743538827248,131.741581108372,132.739623389496,133.069633257233),
 .UNSPECIFIED.);
#433=B_SPLINE_CURVE_WITH_KNOTS('',3,(#15554,#15555,#15556,#15557,#15558,
#15559,#15560,#15561,#15562,#15563,#15564,#15565,#15566,#15567,#15568,#15569,
#15570,#15571,#15572,#15573,#15574,#15575),.UNSPECIFIED.,.F.,.F.,(4,3,3,
3,3,3,3,4),(-142.322100278399,-141.665286242036,-140.667643381176,-139.670000520317,
-138.672357659457,-137.674714798598,-136.677071937739,-136.03891497122),
 .UNSPECIFIED.);
#434=B_SPLINE_CURVE_WITH_KNOTS('',3,(#15576,#15577,#15578,#15579,#15580,
#15581,#15582,#15583,#15584,#15585,#15586,#15587,#15588,#15589,#15590,#15591,
#15592,#15593,#15594,#15595,#15596,#15597),.UNSPECIFIED.,.F.,.F.,(4,3,3,
3,3,3,3,4),(133.069633257233,133.73766567062,134.735707951744,135.733750232868,
136.731792513992,137.729834795116,138.72787707624,139.352818564412),
 .UNSPECIFIED.);
#435=B_SPLINE_CURVE_WITH_KNOTS('',3,(#15602,#15603,#15604,#15605,#15606,
#15607,#15608,#15609,#15610,#15611,#15612,#15613,#15614,#15615,#15616,#15617,
#15618,#15619,#15620,#15621,#15622,#15623),.UNSPECIFIED.,.F.,.F.,(4,3,3,
3,3,3,3,4),(-148.605285585579,-147.651143407192,-146.653500546333,-145.655857685473,
-144.658214824614,-143.660571963754,-142.662929102895,-142.322100278399),
 .UNSPECIFIED.);
#436=B_SPLINE_CURVE_WITH_KNOTS('',3,(#15624,#15625,#15626,#15627,#15628,
#15629,#15630,#15631,#15632,#15633,#15634,#15635,#15636,#15637,#15638,#15639,
#15640,#15641,#15642,#15643,#15644,#15645),.UNSPECIFIED.,.F.,.F.,(4,3,3,
3,3,3,3,4),(139.352818564412,139.725919357364,140.723961638488,141.722003919612,
142.720046200736,143.71808848186,144.716130762984,145.636003871592),
 .UNSPECIFIED.);
#437=B_SPLINE_CURVE_WITH_KNOTS('',3,(#15650,#15651,#15652,#15653,#15654,
#15655,#15656,#15657,#15658,#15659,#15660,#15661,#15662,#15663,#15664,#15665,
#15666,#15667,#15668,#15669,#15670,#15671,#15672,#15673,#15674),
 .UNSPECIFIED.,.F.,.F.,(4,3,3,3,3,3,3,3,4),(-154.888470892759,-154.634643433208,
-153.637000572349,-152.639357711489,-151.64171485063,-150.64407198977,-149.646429128911,
-148.648786268052,-148.605285585579),.UNSPECIFIED.);
#438=B_SPLINE_CURVE_WITH_KNOTS('',3,(#15675,#15676,#15677,#15678,#15679,
#15680,#15681,#15682,#15683,#15684,#15685,#15686,#15687,#15688,#15689,#15690,
#15691,#15692,#15693,#15694,#15695,#15696,#15697,#15698,#15699),
 .UNSPECIFIED.,.F.,.F.,(4,3,3,3,3,3,3,3,4),(145.636003871592,145.714173044108,
146.712215325232,147.710257606356,148.70829988748,149.706342168604,150.704384449728,
151.702426730852,151.919189178771),.UNSPECIFIED.);
#439=B_SPLINE_CURVE_WITH_KNOTS('',3,(#15704,#15705,#15706,#15707,#15708,
#15709,#15710,#15711,#15712,#15713,#15714,#15715,#15716,#15717,#15718,#15719,
#15720,#15721,#15722,#15723,#15724,#15725),.UNSPECIFIED.,.F.,.F.,(4,3,3,
3,3,3,3,4),(-161.171656199938,-160.620500598364,-159.622857737505,-158.625214876646,
-157.627572015786,-156.629929154927,-155.632286294067,-154.888470892759),
 .UNSPECIFIED.);
#440=B_SPLINE_CURVE_WITH_KNOTS('',3,(#15726,#15727,#15728,#15729,#15730,
#15731,#15732,#15733,#15734,#15735,#15736,#15737,#15738,#15739,#15740,#15741,
#15742,#15743,#15744,#15745,#15746,#15747),.UNSPECIFIED.,.F.,.F.,(4,3,3,
3,3,3,3,4),(151.919189178771,152.700469011976,153.6985112931,154.696553574224,
155.694595855348,156.692638136472,157.690680417596,158.202374485951),
 .UNSPECIFIED.);
#441=B_SPLINE_CURVE_WITH_KNOTS('',3,(#15752,#15753,#15754,#15755,#15756,
#15757,#15758,#15759,#15760,#15761,#15762,#15763,#15764,#15765,#15766,#15767,
#15768,#15769,#15770,#15771,#15772,#15773),.UNSPECIFIED.,.F.,.F.,(4,3,3,
3,3,3,3,4),(-167.454841507118,-166.606357763521,-165.608714902661,-164.611072041802,
-163.613429180943,-162.615786320083,-161.618143459224,-161.171656199938),
 .UNSPECIFIED.);
#442=B_SPLINE_CURVE_WITH_KNOTS('',3,(#15774,#15775,#15776,#15777,#15778,
#15779,#15780,#15781,#15782,#15783,#15784,#15785,#15786,#15787,#15788,#15789,
#15790,#15791,#15792,#15793,#15794,#15795),.UNSPECIFIED.,.F.,.F.,(4,3,3,
3,3,3,3,4),(158.202374485951,158.68872269872,159.686764979844,160.684807260968,
161.682849542092,162.680891823216,163.67893410434,164.48555979313),
 .UNSPECIFIED.);
#443=B_SPLINE_CURVE_WITH_KNOTS('',3,(#15800,#15801,#15802,#15803,#15804,
#15805,#15806,#15807,#15808,#15809,#15810,#15811,#15812,#15813,#15814,#15815,
#15816,#15817,#15818,#15819,#15820,#15821,#15822,#15823,#15824),
 .UNSPECIFIED.,.F.,.F.,(4,3,3,3,3,3,3,3,4),(-173.738026814297,-173.589857789537,
-172.592214928677,-171.594572067818,-170.596929206958,-169.599286346099,
-168.60164348524,-167.60400062438,-167.454841507118),.UNSPECIFIED.);
#444=B_SPLINE_CURVE_WITH_KNOTS('',3,(#15825,#15826,#15827,#15828,#15829,
#15830,#15831,#15832,#15833,#15834,#15835,#15836,#15837,#15838,#15839,#15840,
#15841,#15842,#15843,#15844,#15845,#15846,#15847,#15848,#15849),
 .UNSPECIFIED.,.F.,.F.,(4,3,3,3,3,3,3,3,4),(164.48555979313,164.676976385465,
165.675018666588,166.673060947713,167.671103228837,168.669145509961,169.667187791085,
170.665230072209,170.76874510031),.UNSPECIFIED.);
#445=B_SPLINE_CURVE_WITH_KNOTS('',3,(#15854,#15855,#15856,#15857,#15858,
#15859,#15860,#15861,#15862,#15863,#15864,#15865,#15866,#15867,#15868,#15869,
#15870,#15871,#15872,#15873,#15874,#15875),.UNSPECIFIED.,.F.,.F.,(4,3,3,
3,3,3,3,4),(-180.021212121477,-179.575714954693,-178.578072093834,-177.580429232974,
-176.582786372115,-175.585143511255,-174.587500650396,-173.738026814297),
 .UNSPECIFIED.);
#446=B_SPLINE_CURVE_WITH_KNOTS('',3,(#15876,#15877,#15878,#15879,#15880,
#15881,#15882,#15883,#15884,#15885,#15886,#15887,#15888,#15889,#15890,#15891,
#15892,#15893,#15894,#15895,#15896,#15897),.UNSPECIFIED.,.F.,.F.,(4,3,3,
3,3,3,3,4),(170.76874510031,171.663272353333,172.661314634457,173.659356915581,
174.657399196705,175.655441477829,176.653483758953,177.051930407489),
 .UNSPECIFIED.);
#447=B_SPLINE_CURVE_WITH_KNOTS('',3,(#15902,#15903,#15904,#15905,#15906,
#15907,#15908,#15909,#15910,#15911,#15912,#15913,#15914,#15915,#15916,#15917,
#15918,#15919,#15920,#15921,#15922,#15923),.UNSPECIFIED.,.F.,.F.,(4,3,3,
3,3,3,3,4),(-186.304397428656,-185.56157211985,-184.56392925899,-183.566286398131,
-182.568643537271,-181.571000676412,-180.573357815553,-180.021212121477),
 .UNSPECIFIED.);
#448=B_SPLINE_CURVE_WITH_KNOTS('',3,(#15924,#15925,#15926,#15927,#15928,
#15929,#15930,#15931,#15932,#15933,#15934,#15935,#15936,#15937,#15938,#15939,
#15940,#15941,#15942,#15943,#15944,#15945),.UNSPECIFIED.,.F.,.F.,(4,3,3,
3,3,3,3,4),(177.051930407489,177.651526040077,178.649568321201,179.647610602325,
180.645652883449,181.643695164573,182.641737445697,183.335115714669),
 .UNSPECIFIED.);
#449=B_SPLINE_CURVE_WITH_KNOTS('',3,(#15951,#15952,#15953,#15954,#15955,
#15956,#15957,#15958,#15959,#15960),.UNSPECIFIED.,.F.,.F.,(4,1,1,1,1,1,
1,4),(197.920337176157,198.17515472821,199.172797589069,200.170440449928,
201.168083310788,202.165726171647,203.163369032507,204.161011893366),
 .UNSPECIFIED.);
#450=B_SPLINE_CURVE_WITH_KNOTS('',3,(#15963,#15964,#15965,#15966,#15967,
#15968,#15969,#15970,#15971),.UNSPECIFIED.,.F.,.F.,(4,1,1,1,1,1,4),(197.920337176157,
197.930069567874,198.928111848998,199.926154130122,200.924196411246,201.92223869237,
202.920280973494),.UNSPECIFIED.);
#451=B_SPLINE_CURVE_WITH_KNOTS('',3,(#15976,#15977,#15978,#15979,#15980,
#15981,#15982,#15983,#15984,#15985),.UNSPECIFIED.,.F.,.F.,(4,1,1,1,1,1,
1,4),(191.637151868977,192.189297563053,193.186940423913,194.184583284772,
195.182226145631,196.179869006491,197.17751186735,197.920337176157),
 .UNSPECIFIED.);
#452=B_SPLINE_CURVE_WITH_KNOTS('',3,(#15986,#15987,#15988,#15989,#15990,
#15991,#15992,#15993,#15994,#15995),.UNSPECIFIED.,.F.,.F.,(4,1,1,1,1,1,
1,4),(191.637151868977,191.94181588113,192.939858162254,193.937900443378,
194.935942724502,195.933985005626,196.93202728675,197.920337176157),
 .UNSPECIFIED.);
#453=B_SPLINE_CURVE_WITH_KNOTS('',3,(#16000,#16001,#16002,#16003,#16004,
#16005,#16006,#16007,#16008,#16009),.UNSPECIFIED.,.F.,.F.,(4,1,1,1,1,1,
1,4),(185.353966561798,186.203440397897,187.201083258756,188.198726119616,
189.196368980475,190.194011841334,191.191654702194,191.637151868977),
 .UNSPECIFIED.);
#454=B_SPLINE_CURVE_WITH_KNOTS('',3,(#16010,#16011,#16012,#16013,#16014,
#16015,#16016,#16017,#16018,#16019),.UNSPECIFIED.,.F.,.F.,(4,1,1,1,1,1,
1,4),(185.353966561798,185.953562194385,186.951604475509,187.949646756633,
188.947689037757,189.945731318881,190.943773600006,191.637151868977),
 .UNSPECIFIED.);
#455=B_SPLINE_CURVE_WITH_KNOTS('',3,(#16024,#16025,#16026,#16027,#16028,
#16029,#16030,#16031,#16032,#16033,#16034),.UNSPECIFIED.,.F.,.F.,(4,1,1,
1,1,1,1,1,4),(179.070781254618,179.219940371881,180.21758323274,181.2152260936,
182.212868954459,183.210511815318,184.208154676178,185.205797537037,185.353966561798),
 .UNSPECIFIED.);
#456=B_SPLINE_CURVE_WITH_KNOTS('',3,(#16035,#16036,#16037,#16038,#16039,
#16040,#16041,#16042,#16043,#16044),.UNSPECIFIED.,.F.,.F.,(4,1,1,1,1,1,
1,4),(179.070781254618,179.965308507641,180.963350788765,181.961393069889,
182.959435351013,183.957477632137,184.955519913261,185.353966561798),
 .UNSPECIFIED.);
#457=B_SPLINE_CURVE_WITH_KNOTS('',3,(#16049,#16050,#16051,#16052,#16053,
#16054,#16055,#16056,#16057,#16058),.UNSPECIFIED.,.F.,.F.,(4,1,1,1,1,1,
1,4),(172.787595947439,173.234083206724,174.231726067584,175.229368928443,
176.227011789303,177.224654650162,178.222297511021,179.070781254618),
 .UNSPECIFIED.);
#458=B_SPLINE_CURVE_WITH_KNOTS('',3,(#16059,#16060,#16061,#16062,#16063,
#16064,#16065,#16066,#16067,#16068,#16069),.UNSPECIFIED.,.F.,.F.,(4,1,1,
1,1,1,1,1,4),(172.787595947439,172.979012539773,173.977054820897,174.975097102021,
175.973139383145,176.971181664269,177.969223945393,178.967266226517,179.070781254618),
 .UNSPECIFIED.);
#459=B_SPLINE_CURVE_WITH_KNOTS('',3,(#16074,#16075,#16076,#16077,#16078,
#16079,#16080,#16081,#16082,#16083),.UNSPECIFIED.,.F.,.F.,(4,1,1,1,1,1,
1,4),(166.504410640259,167.248226041568,168.245868902427,169.243511763287,
170.241154624146,171.238797485006,172.236440345865,172.787595947439),
 .UNSPECIFIED.);
#460=B_SPLINE_CURVE_WITH_KNOTS('',3,(#16084,#16085,#16086,#16087,#16088,
#16089,#16090,#16091,#16092,#16093),.UNSPECIFIED.,.F.,.F.,(4,1,1,1,1,1,
1,4),(166.504410640259,166.990758853029,167.988801134153,168.986843415277,
169.984885696401,170.982927977525,171.980970258649,172.787595947439),
 .UNSPECIFIED.);
#461=B_SPLINE_CURVE_WITH_KNOTS('',3,(#16098,#16099,#16100,#16101,#16102,
#16103,#16104,#16105,#16106,#16107,#16108),.UNSPECIFIED.,.F.,.F.,(4,1,1,
1,1,1,1,1,4),(160.22122533308,160.264726015552,161.262368876412,162.260011737271,
163.25765459813,164.25529745899,165.252940319849,166.250583180709,166.504410640259),
 .UNSPECIFIED.);
#462=B_SPLINE_CURVE_WITH_KNOTS('',3,(#16109,#16110,#16111,#16112,#16113,
#16114,#16115,#16116,#16117,#16118),.UNSPECIFIED.,.F.,.F.,(4,1,1,1,1,1,
1,4),(160.22122533308,161.002505166285,162.000547447409,162.998589728533,
163.996632009657,164.994674290781,165.992716571905,166.504410640259),
 .UNSPECIFIED.);
#463=B_SPLINE_CURVE_WITH_KNOTS('',3,(#16123,#16124,#16125,#16126,#16127,
#16128,#16129,#16130,#16131,#16132),.UNSPECIFIED.,.F.,.F.,(4,1,1,1,1,1,
1,4),(153.9380400259,154.278868850396,155.276511711255,156.274154572115,
157.271797432974,158.269440293833,159.267083154693,160.22122533308),
 .UNSPECIFIED.);
#464=B_SPLINE_CURVE_WITH_KNOTS('',3,(#16133,#16134,#16135,#16136,#16137,
#16138,#16139,#16140,#16141,#16142,#16143),.UNSPECIFIED.,.F.,.F.,(4,1,1,
1,1,1,1,1,4),(153.9380400259,154.016209198417,155.014251479541,156.012293760665,
157.010336041789,158.008378322913,159.006420604037,160.004462885161,160.22122533308),
 .UNSPECIFIED.);
#465=B_SPLINE_CURVE_WITH_KNOTS('',3,(#16148,#16149,#16150,#16151,#16152,
#16153,#16154,#16155,#16156,#16157),.UNSPECIFIED.,.F.,.F.,(4,1,1,1,1,1,
1,4),(147.65485471872,148.293011685239,149.290654546099,150.288297406958,
151.285940267817,152.283583128677,153.281225989536,153.9380400259),
 .UNSPECIFIED.);
#466=B_SPLINE_CURVE_WITH_KNOTS('',3,(#16158,#16159,#16160,#16161,#16162,
#16163,#16164,#16165,#16166,#16167),.UNSPECIFIED.,.F.,.F.,(4,1,1,1,1,1,
1,4),(147.65485471872,148.027955511672,149.025997792796,150.02404007392,
151.022082355044,152.020124636168,153.018166917292,153.9380400259),
 .UNSPECIFIED.);
#467=B_SPLINE_CURVE_WITH_KNOTS('',3,(#16172,#16173,#16174,#16175,#16176,
#16177,#16178,#16179,#16180,#16181),.UNSPECIFIED.,.F.,.F.,(4,1,1,1,1,1,
1,4),(141.371669411541,142.307154520083,143.304797380942,144.302440241802,
145.300083102661,146.29772596352,147.29536882438,147.65485471872),
 .UNSPECIFIED.);
#468=B_SPLINE_CURVE_WITH_KNOTS('',3,(#16182,#16183,#16184,#16185,#16186,
#16187,#16188,#16189,#16190,#16191),.UNSPECIFIED.,.F.,.F.,(4,1,1,1,1,1,
1,4),(141.371669411541,142.039701824928,143.037744106052,144.035786387176,
145.0338286683,146.031870949424,147.029913230548,147.65485471872),
 .UNSPECIFIED.);
#469=B_SPLINE_CURVE_WITH_KNOTS('',3,(#16196,#16197,#16198,#16199,#16200,
#16201,#16202,#16203,#16204,#16205,#16206),.UNSPECIFIED.,.F.,.F.,(4,1,1,
1,1,1,1,1,4),(135.088484104361,135.323654494067,136.321297354926,137.318940215786,
138.316583076645,139.314225937505,140.311868798364,141.309511659223,141.371669411541),
 .UNSPECIFIED.);
#470=B_SPLINE_CURVE_WITH_KNOTS('',3,(#16207,#16208,#16209,#16210,#16211,
#16212,#16213,#16214,#16215,#16216),.UNSPECIFIED.,.F.,.F.,(4,1,1,1,1,1,
1,4),(135.088484104361,136.051448138184,137.049490419308,138.047532700432,
139.045574981556,140.04361726268,141.041659543804,141.371669411541),
 .UNSPECIFIED.);
#471=B_SPLINE_CURVE_WITH_KNOTS('',3,(#16221,#16222,#16223,#16224,#16225,
#16226,#16227,#16228,#16229,#16230),.UNSPECIFIED.,.F.,.F.,(4,1,1,1,1,1,
1,4),(128.805298797182,129.337797328911,130.33544018977,131.333083050629,
132.330725911489,133.328368772348,134.326011633208,135.088484104361),
 .UNSPECIFIED.);
#472=B_SPLINE_CURVE_WITH_KNOTS('',3,(#16231,#16232,#16233,#16234,#16235,
#16236,#16237,#16238,#16239,#16240,#16241),.UNSPECIFIED.,.F.,.F.,(4,1,1,
1,1,1,1,1,4),(128.805298797182,129.065152170316,130.06319445144,131.061236732564,
132.059279013688,133.057321294812,134.055363575936,135.05340585706,135.088484104361),
 .UNSPECIFIED.);
#473=B_SPLINE_CURVE_WITH_KNOTS('',3,(#16246,#16247,#16248,#16249,#16250,
#16251,#16252,#16253,#16254,#16255),.UNSPECIFIED.,.F.,.F.,(4,1,1,1,1,1,
1,4),(122.522113490002,123.351940163754,124.349583024614,125.347225885473,
126.344868746332,127.342511607192,128.340154468051,128.805298797182),
 .UNSPECIFIED.);
#474=B_SPLINE_CURVE_WITH_KNOTS('',3,(#16256,#16257,#16258,#16259,#16260,
#16261,#16262,#16263,#16264,#16265),.UNSPECIFIED.,.F.,.F.,(4,1,1,1,1,1,
1,4),(122.522113490002,123.076898483572,124.074940764696,125.07298304582,
126.071025326944,127.069067608068,128.067109889192,128.805298797182),
 .UNSPECIFIED.);
#475=B_SPLINE_CURVE_WITH_KNOTS('',3,(#16270,#16271,#16272,#16273,#16274,
#16275,#16276,#16277,#16278,#16279,#16280),.UNSPECIFIED.,.F.,.F.,(4,1,1,
1,1,1,1,1,4),(116.238928182823,116.368440137738,117.366082998598,118.363725859457,
119.361368720316,120.359011581176,121.356654442035,122.354297302895,122.522113490002),
 .UNSPECIFIED.);
#476=B_SPLINE_CURVE_WITH_KNOTS('',3,(#16281,#16282,#16283,#16284,#16285,
#16286,#16287,#16288,#16289,#16290),.UNSPECIFIED.,.F.,.F.,(4,1,1,1,1,1,
1,4),(116.238928182823,117.088644796828,118.086687077952,119.084729359076,
120.0827716402,121.080813921324,122.078856202448,122.522113490002),
 .UNSPECIFIED.);
#477=B_SPLINE_CURVE_WITH_KNOTS('',3,(#16295,#16296,#16297,#16298,#16299,
#16300,#16301,#16302,#16303,#16304),.UNSPECIFIED.,.F.,.F.,(4,1,1,1,1,1,
1,4),(109.955742875643,110.382582972582,111.380225833441,112.377868694301,
113.37551155516,114.373154416019,115.370797276879,116.238928182823),
 .UNSPECIFIED.);
#478=B_SPLINE_CURVE_WITH_KNOTS('',3,(#16305,#16306,#16307,#16308,#16309,
#16310,#16311,#16312,#16313,#16314,#16315),.UNSPECIFIED.,.F.,.F.,(4,1,1,
1,1,1,1,1,4),(109.955742875643,110.102348828959,111.100391110083,112.098433391207,
113.096475672331,114.094517953455,115.092560234579,116.090602515703,116.238928182823),
 .UNSPECIFIED.);
#479=B_SPLINE_CURVE_WITH_KNOTS('',3,(#16320,#16321,#16322,#16323,#16324,
#16325,#16326,#16327,#16328,#16329),.UNSPECIFIED.,.F.,.F.,(4,1,1,1,1,1,
1,4),(103.672557568463,104.396725807425,105.394368668285,106.392011529144,
107.389654390004,108.387297250863,109.384940111722,109.955742875643),
 .UNSPECIFIED.);
#480=B_SPLINE_CURVE_WITH_KNOTS('',3,(#16330,#16331,#16332,#16333,#16334,
#16335,#16336,#16337,#16338,#16339),.UNSPECIFIED.,.F.,.F.,(4,1,1,1,1,1,
1,4),(103.672557568463,104.114095142215,105.112137423339,106.110179704463,
107.108221985587,108.106264266711,109.104306547835,109.955742875643),
 .UNSPECIFIED.);
#481=B_SPLINE_CURVE_WITH_KNOTS('',3,(#16344,#16345,#16346,#16347,#16348,
#16349,#16350,#16351,#16352,#16353,#16354),.UNSPECIFIED.,.F.,.F.,(4,1,1,
1,1,1,1,1,4),(97.3893722612837,97.4132257814096,98.410868642269,99.4085115031284,
100.406154363988,101.403797224847,102.401440085707,103.399082946566,103.672557568463),
 .UNSPECIFIED.);
#482=B_SPLINE_CURVE_WITH_KNOTS('',3,(#16355,#16356,#16357,#16358,#16359,
#16360,#16361,#16362,#16363,#16364),.UNSPECIFIED.,.F.,.F.,(4,1,1,1,1,1,
1,4),(97.3893722612838,98.125841455471,99.123883736595,100.121926017719,
101.119968298843,102.118010579967,103.116052861091,103.672557568463),
 .UNSPECIFIED.);
#483=B_SPLINE_CURVE_WITH_KNOTS('',3,(#16369,#16370,#16371,#16372,#16373,
#16374,#16375,#16376,#16377,#16378),.UNSPECIFIED.,.F.,.F.,(4,1,1,1,1,1,
1,4),(91.1061869541041,91.4273686162531,92.4250114771125,93.4226543379719,
94.4202971988313,95.4179400596907,96.4155829205502,97.3893722612837),
 .UNSPECIFIED.);
#484=B_SPLINE_CURVE_WITH_KNOTS('',3,(#16379,#16380,#16381,#16382,#16383,
#16384,#16385,#16386,#16387,#16388,#16389),.UNSPECIFIED.,.F.,.F.,(4,1,1,
1,1,1,1,1,4),(91.1061869541042,91.1395454876028,92.1375877687268,93.1356300498508,
94.1336723309749,95.1317146120989,96.1297568932229,97.127799174347,97.3893722612838),
 .UNSPECIFIED.);
#485=B_SPLINE_CURVE_WITH_KNOTS('',3,(#16394,#16395,#16396,#16397,#16398,
#16399,#16400,#16401,#16402,#16403),.UNSPECIFIED.,.F.,.F.,(4,1,1,1,1,1,
1,4),(84.8230016469245,85.4415114510967,86.4391543119561,87.4367971728155,
88.4344400336749,89.4320828945343,90.4297257553937,91.1061869541041),
 .UNSPECIFIED.);
#486=B_SPLINE_CURVE_WITH_KNOTS('',3,(#16404,#16405,#16406,#16407,#16408,
#16409,#16410,#16411,#16412,#16413),.UNSPECIFIED.,.F.,.F.,(4,1,1,1,1,1,
1,4),(84.8230016469246,85.1512918008586,86.1493340819827,87.1473763631067,
88.1454186442307,89.1434609253548,90.1415032064788,91.1061869541042),
 .UNSPECIFIED.);
#487=B_SPLINE_CURVE_WITH_KNOTS('',3,(#16418,#16419,#16420,#16421,#16422,
#16423,#16424,#16425,#16426,#16427),.UNSPECIFIED.,.F.,.F.,(4,1,1,1,1,1,
1,4),(78.539816339745,79.4556542859402,80.4532971467996,81.4509400076591,
82.4485828685185,83.4462257293779,84.4438685902373,84.8230016469245),
 .UNSPECIFIED.);
#488=B_SPLINE_CURVE_WITH_KNOTS('',3,(#16428,#16429,#16430,#16431,#16432,
#16433,#16434,#16435,#16436,#16437),.UNSPECIFIED.,.F.,.F.,(4,1,1,1,1,1,
1,4),(78.539816339745,79.1630381141145,80.1610803952385,81.1591226763625,
82.1571649574865,83.1552072386106,84.1532495197346,84.8230016469246),
 .UNSPECIFIED.);
#489=B_SPLINE_CURVE_WITH_KNOTS('',3,(#16442,#16443,#16444,#16445,#16446,
#16447,#16448,#16449,#16450,#16451,#16452),.UNSPECIFIED.,.F.,.F.,(4,1,1,
1,1,1,1,1,4),(72.2566310325654,72.4721542599244,73.4697971207838,74.4674399816432,
75.4650828425026,76.462725703362,77.4603685642214,78.4580114250808,78.539816339745),
 .UNSPECIFIED.);
#490=B_SPLINE_CURVE_WITH_KNOTS('',3,(#16453,#16454,#16455,#16456,#16457,
#16458,#16459,#16460,#16461,#16462),.UNSPECIFIED.,.F.,.F.,(4,1,1,1,1,1,
1,4),(72.2566310325654,73.1747844273703,74.1728267084943,75.1708689896184,
76.1689112707424,77.1669535518664,78.1649958329905,78.539816339745),
 .UNSPECIFIED.);
#491=B_SPLINE_CURVE_WITH_KNOTS('',3,(#16467,#16468,#16469,#16470,#16471,
#16472,#16473,#16474,#16475,#16476),.UNSPECIFIED.,.F.,.F.,(4,1,1,1,1,1,
1,4),(65.9734457253858,66.486297094768,67.4839399556274,68.4815828164868,
69.4792256773462,70.4768685382056,71.474511399065,72.2566310325654),
 .UNSPECIFIED.);
#492=B_SPLINE_CURVE_WITH_KNOTS('',3,(#16477,#16478,#16479,#16480,#16481,
#16482,#16483,#16484,#16485,#16486,#16487),.UNSPECIFIED.,.F.,.F.,(4,1,1,
1,1,1,1,1,4),(65.9734457253858,66.1884884595021,67.1865307406262,68.1845730217502,
69.1826153028742,70.1806575839982,71.1786998651223,72.1767421462463,72.2566310325654),
 .UNSPECIFIED.);
#493=B_SPLINE_CURVE_WITH_KNOTS('',3,(#16492,#16493,#16494,#16495,#16496,
#16497,#16498,#16499,#16500,#16501),.UNSPECIFIED.,.F.,.F.,(4,1,1,1,1,1,
1,4),(59.6902604182062,60.5004399296115,61.4980827904709,62.4957256513303,
63.4933685121897,64.4910113730492,65.4886542339086,65.9734457253858),
 .UNSPECIFIED.);
#494=B_SPLINE_CURVE_WITH_KNOTS('',3,(#16502,#16503,#16504,#16505,#16506,
#16507,#16508,#16509,#16510,#16511),.UNSPECIFIED.,.F.,.F.,(4,1,1,1,1,1,
1,4),(59.6902604182062,60.200234772758,61.198277053882,62.196319335006,
63.19436161613,64.1924038972541,65.1904461783781,65.9734457253858),
 .UNSPECIFIED.);
#495=B_SPLINE_CURVE_WITH_KNOTS('',3,(#16516,#16517,#16518,#16519,#16520,
#16521,#16522,#16523,#16524,#16525,#16526),.UNSPECIFIED.,.F.,.F.,(4,1,1,
1,1,1,1,1,4),(53.4070751110266,53.5169399035957,54.5145827644551,55.5122256253145,
56.5098684861739,57.5075113470333,58.5051542078927,59.5027970687521,59.6902604182062),
 .UNSPECIFIED.);
#496=B_SPLINE_CURVE_WITH_KNOTS('',3,(#16527,#16528,#16529,#16530,#16531,
#16532,#16533,#16534,#16535,#16536),.UNSPECIFIED.,.F.,.F.,(4,1,1,1,1,1,
1,4),(53.4070751110266,54.2119810860138,55.2100233671378,56.2080656482619,
57.2061079293859,58.2041502105099,59.2021924916339,59.6902604182062),
 .UNSPECIFIED.);
#497=B_SPLINE_CURVE_WITH_KNOTS('',3,(#16541,#16542,#16543,#16544,#16545,
#16546,#16547,#16548,#16549,#16550),.UNSPECIFIED.,.F.,.F.,(4,1,1,1,1,1,
1,4),(47.123889803847,47.5310827384393,48.5287255992987,49.5263684601581,
50.5240113210175,51.5216541818769,52.5192970427363,53.4070751110266),
 .UNSPECIFIED.);
#498=B_SPLINE_CURVE_WITH_KNOTS('',3,(#16551,#16552,#16553,#16554,#16555,
#16556,#16557,#16558,#16559,#16560,#16561),.UNSPECIFIED.,.F.,.F.,(4,1,1,
1,1,1,1,1,4),(47.123889803847,47.2256851181456,48.2237273992696,49.2217696803937,
50.2198119615177,51.2178542426417,52.2158965237657,53.2139388048898,53.4070751110266),
 .UNSPECIFIED.);
#499=B_SPLINE_CURVE_WITH_KNOTS('',3,(#16566,#16567,#16568,#16569,#16570,
#16571,#16572,#16573,#16574,#16575),.UNSPECIFIED.,.F.,.F.,(4,1,1,1,1,1,
1,4),(40.8407044966674,41.5452255732828,42.5428684341422,43.5405112950016,
44.538154155861,45.5357970167204,46.5334398775799,47.123889803847),
 .UNSPECIFIED.);
#500=B_SPLINE_CURVE_WITH_KNOTS('',3,(#16576,#16577,#16578,#16579,#16580,
#16581,#16582,#16583,#16584,#16585),.UNSPECIFIED.,.F.,.F.,(4,1,1,1,1,1,
1,4),(40.8407044966675,41.2374314314014,42.2354737125255,43.2335159936495,
44.2315582747735,45.2296005558975,46.2276428370216,47.123889803847),
 .UNSPECIFIED.);
#501=B_SPLINE_CURVE_WITH_KNOTS('',3,(#16590,#16591,#16592,#16593,#16594,
#16595,#16596,#16597,#16598,#16599,#16600),.UNSPECIFIED.,.F.,.F.,(4,1,1,
1,1,1,1,1,4),(34.5575191894878,34.561725547267,35.5593684081264,36.5570112689858,
37.5546541298452,38.5522969907046,39.549939851564,40.5475827124234,40.8407044966674),
 .UNSPECIFIED.);
#502=B_SPLINE_CURVE_WITH_KNOTS('',3,(#16601,#16602,#16603,#16604,#16605,
#16606,#16607,#16608,#16609,#16610),.UNSPECIFIED.,.F.,.F.,(4,1,1,1,1,1,
1,4),(34.5575191894879,35.2491777446573,36.2472200257813,37.2452623069053,
38.2433045880294,39.2413468691534,40.2393891502774,40.8407044966675),
 .UNSPECIFIED.);
#503=B_SPLINE_CURVE_WITH_KNOTS('',3,(#16615,#16616,#16617,#16618,#16619,
#16620,#16621,#16622,#16623,#16624),.UNSPECIFIED.,.F.,.F.,(4,1,1,1,1,1,
1,4),(28.2743338823082,28.5758683821105,29.5735112429699,30.5711541038294,
31.5687969646888,32.5664398255482,33.5640826864076,34.5575191894878),
 .UNSPECIFIED.);
#504=B_SPLINE_CURVE_WITH_KNOTS('',3,(#16625,#16626,#16627,#16628,#16629,
#16630,#16631,#16632,#16633,#16634),.UNSPECIFIED.,.F.,.F.,(4,1,1,1,1,1,
1,4),(28.2743338823083,29.2609240579131,30.2589663390371,31.2570086201612,
32.2550509012852,33.2530931824092,34.2511354635333,34.5575191894879),
 .UNSPECIFIED.);
#505=B_SPLINE_CURVE_WITH_KNOTS('',3,(#16639,#16640,#16641,#16642,#16643,
#16644,#16645,#16646,#16647,#16648),.UNSPECIFIED.,.F.,.F.,(4,1,1,1,1,1,
1,4),(21.9911485751286,22.5900112169541,23.5876540778135,24.5852969386729,
25.5829397995323,26.5805826603917,27.5782255212511,28.2743338823082),
 .UNSPECIFIED.);
#506=B_SPLINE_CURVE_WITH_KNOTS('',3,(#16649,#16650,#16651,#16652,#16653,
#16654,#16655,#16656,#16657,#16658,#16659),.UNSPECIFIED.,.F.,.F.,(4,1,1,
1,1,1,1,1,4),(21.9911485751287,22.2746280900449,23.272670371169,24.270712652293,
25.268754933417,26.266797214541,27.2648394956651,28.2628817767891,28.2743338823083),
 .UNSPECIFIED.);
#507=B_SPLINE_CURVE_WITH_KNOTS('',3,(#16664,#16665,#16666,#16667,#16668,
#16669,#16670,#16671,#16672,#16673),.UNSPECIFIED.,.F.,.F.,(4,1,1,1,1,1,
1,4),(15.707963267949,16.6041540517977,17.6017969126571,18.5994397735165,
19.5970826343759,20.5947254952353,21.5923683560947,21.9911485751286),
 .UNSPECIFIED.);
#508=B_SPLINE_CURVE_WITH_KNOTS('',3,(#16674,#16675,#16676,#16677,#16678,
#16679,#16680,#16681,#16682,#16683),.UNSPECIFIED.,.F.,.F.,(4,1,1,1,1,1,
1,4),(15.7079632679491,16.2863744033008,17.2844166844248,18.2824589655488,
19.2805012466728,20.2785435277969,21.2765858089209,21.9911485751287),
 .UNSPECIFIED.);
#509=B_SPLINE_CURVE_WITH_KNOTS('',3,(#16686,#16687,#16688,#16689,#16690,
#16691,#16692,#16693,#16694,#16695,#16696,#16697,#16698,#16699,#16700,#16701,
#16702,#16703,#16704,#16705,#16706,#16707,#16708,#16709,#16710,#16711,#16712,
#16713,#16714,#16715,#16716,#16717,#16718,#16719,#16720,#16721,#16722,#16723,
#16724,#16725,#16726,#16727,#16728,#16729,#16730,#16731,#16732,#16733,#16734,
#16735,#16736,#16737,#16738,#16739,#16740,#16741,#16742,#16743,#16744,#16745,
#16746,#16747,#16748,#16749,#16750,#16751,#16752,#16753,#16754,#16755,#16756,
#16757,#16758,#16759,#16760,#16761,#16762,#16763,#16764,#16765,#16766,#16767,
#16768,#16769,#16770,#16771,#16772,#16773,#16774,#16775,#16776,#16777,#16778,
#16779,#16780,#16781,#16782,#16783,#16784,#16785,#16786,#16787,#16788,#16789,
#16790,#16791,#16792,#16793,#16794,#16795,#16796,#16797,#16798,#16799,#16800,
#16801,#16802,#16803,#16804,#16805,#16806),.UNSPECIFIED.,.F.,.F.,(4,3,3,
3,3,3,3,3,3,3,3,3,3,3,3,3,3,3,3,3,3,3,3,3,3,3,3,3,3,3,3,3,3,3,3,3,3,3,3,
3,4),(-0.753008129282056,-0.726412283548368,-0.715911613874471,-0.694893371653716,
-0.683361029549332,-0.673826434412814,-0.652889016486892,-0.639679181765185,
-0.63195159856097,-0.60480408471638,-0.59150990338668,-0.582561183693184,
-0.554067746128576,-0.540494882749548,-0.528208608719221,-0.505843484121927,
-0.4921308028701,-0.483102814228457,-0.456032674248847,-0.436199115577779,
-0.427073928162626,-0.400948091236321,-0.382860905241332,-0.374822254310016,
-0.34584221065474,-0.333939649620793,-0.324058619604945,-0.29393738163796,
-0.278576588250954,-0.269234263278142,-0.238815915606663,-0.225742435796944,
-0.216239773488962,-0.18666367230127,-0.170750005528772,-0.161294486761502,
-0.129614927749849,-0.114924930935507,-0.106250072717365,-0.0979353687381955,
-0.0965360155478562),.UNSPECIFIED.);
#510=B_SPLINE_CURVE_WITH_KNOTS('',3,(#16808,#16809,#16810,#16811,#16812,
#16813,#16814,#16815,#16816,#16817,#16818,#16819,#16820,#16821,#16822,#16823,
#16824,#16825,#16826,#16827,#16828,#16829,#16830,#16831,#16832,#16833,#16834,
#16835,#16836,#16837,#16838,#16839,#16840,#16841,#16842,#16843,#16844),
 .UNSPECIFIED.,.F.,.F.,(4,3,3,3,3,3,3,3,3,3,3,3,4),(-0.204609524178132,
-0.173922074105667,-0.152149392827302,-0.142793959810126,-0.12983323009626,
-0.11308637627832,-0.0998536142809363,-0.090547498816978,-0.0679106241127335,
-0.0514558350659385,-0.042025593252969,-0.0155529233063705,0.),
 .UNSPECIFIED.);
#511=B_SPLINE_CURVE_WITH_KNOTS('',3,(#16847,#16848,#16849,#16850,#16851,
#16852,#16853,#16854,#16855,#16856,#16857,#16858,#16859,#16860,#16861,#16862),
 .UNSPECIFIED.,.F.,.F.,(4,3,3,3,3,4),(-0.0965360155478562,-0.0724020116608921,
-0.0590232605257019,-0.050388474335024,-0.0186937936910934,0.),
 .UNSPECIFIED.);
#512=B_SPLINE_CURVE_WITH_KNOTS('',3,(#17651,#17652,#17653,#17654,#17655,
#17656,#17657,#17658),.UNSPECIFIED.,.F.,.F.,(4,1,1,1,1,4),(11.6159397475006,
12.61358260836,13.6112254692194,14.6088683300789,15.6065111909383,15.707963267949),
 .UNSPECIFIED.);
#513=B_SPLINE_CURVE_WITH_KNOTS('',3,(#17659,#17660,#17661,#17662,#17663,
#17664,#17665,#17666,#17667,#17668,#17669,#17670,#17671,#17672,#17673,#17674,
#17675,#17676,#17677,#17678,#17679,#17680,#17681,#17682,#17683,#17684,#17685,
#17686,#17687,#17688,#17689,#17690,#17691,#17692,#17693,#17694,#17695,#17696,
#17697,#17698,#17699,#17700,#17701,#17702,#17703,#17704,#17705,#17706,#17707),
 .UNSPECIFIED.,.F.,.F.,(4,3,3,3,3,3,3,3,3,3,3,3,3,3,3,3,4),(-0.275362278356892,
-0.263988733943187,-0.242277787653762,-0.228409792083558,-0.208856161945484,
-0.197709057767663,-0.168075464588018,-0.150222803571495,-0.140083955862437,
-0.125365894046572,-0.0997819296507484,-0.0889593225835958,-0.0667194919376969,
-0.0511923416312717,-0.0404361839568205,-0.0141940669149386,0.),
 .UNSPECIFIED.);
#514=B_SPLINE_CURVE_WITH_KNOTS('',3,(#17708,#17709,#17710,#17711,#17712,
#17713,#17714,#17715,#17716,#17717,#17718,#17719,#17720,#17721,#17722,#17723,
#17724,#17725,#17726),.UNSPECIFIED.,.F.,.F.,(4,3,3,3,3,3,4),(-191.027404416132,
-190.549786424147,-189.552143563287,-188.554500702428,-187.556857841568,
-186.559214980709,-186.304397428656),.UNSPECIFIED.);
#515=B_SPLINE_CURVE_WITH_KNOTS('',3,(#17729,#17730,#17731,#17732,#17733,
#17734,#17735,#17736,#17737),.UNSPECIFIED.,.F.,.F.,(4,1,1,1,1,1,4),(10.3752088276283,
11.2961629976806,12.2942052788047,13.2922475599287,14.2902898410527,15.2883321221767,
15.7079632679491),.UNSPECIFIED.);
#516=B_SPLINE_CURVE_WITH_KNOTS('',3,(#18531,#18532,#18533,#18534,#18535,
#18536,#18537,#18538,#18539,#18540,#18541,#18542,#18543,#18544,#18545,#18546,
#18547,#18548,#18549,#18550,#18551,#18552),.UNSPECIFIED.,.F.,.F.,(4,3,3,
3,3,3,3,4),(183.335115714669,183.639779726821,184.637822007945,185.635864289069,
186.633906570193,187.631948851317,188.629991132441,188.954231742812),
 .UNSPECIFIED.);
#517=B_SPLINE_CURVE_WITH_KNOTS('',3,(#18553,#18554,#18555,#18556,#18557,
#18558,#18559,#18560,#18561,#18562,#18563,#18564,#18565,#18566,#18567,#18568,
#18569,#18570,#18571,#18572,#18573,#18574,#18575,#18576,#18577,#18578,#18579,
#18580,#18581,#18582,#18583,#18584,#18585,#18586,#18587,#18588,#18589,#18590,
#18591,#18592,#18593,#18594,#18595,#18596,#18597,#18598,#18599,#18600,#18601,
#18602,#18603,#18604),.UNSPECIFIED.,.F.,.F.,(4,3,3,3,3,3,3,3,3,3,3,3,3,
3,3,3,3,4),(-0.276631791712714,-0.267404104599176,-0.245529112929484,-0.233826742508505,
-0.212230201958684,-0.201819484750363,-0.173281546649687,-0.162756755581661,
-0.152537502224722,-0.140478169692516,-0.120739781640826,-0.110641775261762,
-0.100726383882944,-0.0755447879122082,-0.0587891884452614,-0.0493012364577666,
-0.0182848522583483,0.),.UNSPECIFIED.);
#518=B_SPLINE_CURVE_WITH_KNOTS('',3,(#18659,#18660,#18661,#18662,#18663,
#18664,#18665),.UNSPECIFIED.,.F.,.F.,(4,3,4),(-30.159289474462,-29.2544199692899,
-28.9853432330879),.UNSPECIFIED.);
#519=B_SPLINE_CURVE_WITH_KNOTS('',3,(#18671,#18672,#18673,#18674,#18675,
#18676,#18677,#18678,#18679,#18680,#18681,#18682,#18683,#18684,#18685,#18686,
#18687,#18688,#18689),.UNSPECIFIED.,.F.,.F.,(4,3,3,3,3,3,4),(26.4423043696954,
27.3041253046706,28.2792726369803,29.25441996929,30.2295673015996,31.2047146339093,
32.179861966219),.UNSPECIFIED.);
#520=B_SPLINE_CURVE_WITH_KNOTS('',3,(#18691,#18692,#18693,#18694,#18695,
#18696,#18697,#18698,#18699,#18700,#18701,#18702,#18703,#18704,#18705,#18706,
#18707,#18708,#18709,#18710,#18711,#18712),.UNSPECIFIED.,.F.,.F.,(4,3,3,
3,3,3,3,4),(-28.9853432330879,-28.2792726369803,-27.3041253046706,-26.3289779723609,
-25.3538306400513,-24.3786833077416,-23.403535975432,-22.7021579259084),
 .UNSPECIFIED.);
#521=B_SPLINE_CURVE_WITH_KNOTS('',3,(#18717,#18718,#18719,#18720,#18721,
#18722,#18723,#18724,#18725,#18726,#18727,#18728,#18729,#18730,#18731,#18732,
#18733,#18734,#18735,#18736,#18737,#18738,#18739,#18740,#18741),
 .UNSPECIFIED.,.F.,.F.,(4,3,3,3,3,3,3,3,4),(20.1591190625159,20.478093978503,
21.4532413108126,22.4283886431223,23.403535975432,24.3786833077416,25.3538306400513,
26.328977972361,26.4423043696954),.UNSPECIFIED.);
#522=B_SPLINE_CURVE_WITH_KNOTS('',3,(#18742,#18743,#18744,#18745,#18746,
#18747,#18748,#18749,#18750,#18751,#18752,#18753,#18754,#18755,#18756,#18757,
#18758,#18759,#18760,#18761,#18762,#18763,#18764,#18765,#18766),
 .UNSPECIFIED.,.F.,.F.,(4,3,3,3,3,3,3,3,4),(-22.7021579259084,-22.4283886431223,
-21.4532413108126,-20.478093978503,-19.5029466461933,-18.5277993138836,
-17.552651981574,-16.5775046492643,-16.4189726187288),.UNSPECIFIED.);
#523=B_SPLINE_CURVE_WITH_KNOTS('',3,(#18771,#18772,#18773,#18774,#18775,
#18776,#18777,#18778,#18779,#18780,#18781,#18782,#18783,#18784,#18785,#18786,
#18787,#18788,#18789,#18790,#18791,#18792),.UNSPECIFIED.,.F.,.F.,(4,3,3,
3,3,3,3,4),(13.8759337553363,14.627209984645,15.6023573169546,16.5775046492643,
17.552651981574,18.5277993138836,19.5029466461933,20.1591190625159),
 .UNSPECIFIED.);
#524=B_SPLINE_CURVE_WITH_KNOTS('',3,(#18793,#18794,#18795,#18796,#18797,
#18798,#18799,#18800,#18801,#18802,#18803,#18804,#18805,#18806,#18807,#18808,
#18809,#18810,#18811,#18812,#18813,#18814),.UNSPECIFIED.,.F.,.F.,(4,3,3,
3,3,3,3,4),(-16.4189726187288,-15.6023573169546,-14.627209984645,-13.6520626523353,
-12.6769153200256,-11.701767987716,-10.7266206554063,-10.1357873115492),
 .UNSPECIFIED.);
#525=B_SPLINE_CURVE_WITH_KNOTS('',3,(#18820,#18821,#18822,#18823,#18824,
#18825,#18826,#18827,#18828,#18829,#18830,#18831,#18832),.UNSPECIFIED.,
 .F.,.F.,(4,3,3,3,4),(-3.8526020043696,-2.92544199692899,-1.95029466461933,
-0.975147332309664,0.),.UNSPECIFIED.);
#526=B_SPLINE_CURVE_WITH_KNOTS('',3,(#18835,#18836,#18837,#18838,#18839,
#18840,#18841,#18842,#18843,#18844,#18845,#18846,#18847,#18848,#18849,#18850,
#18851,#18852,#18853),.UNSPECIFIED.,.F.,.F.,(4,3,3,3,3,3,4),(2.02057249175693,
2.925441996929,3.90058932923866,4.87573666154832,5.85088399385799,6.82603132616766,
7.59274844815668),.UNSPECIFIED.);
#527=B_SPLINE_CURVE_WITH_KNOTS('',3,(#18859,#18860,#18861,#18862,#18863,
#18864,#18865),.UNSPECIFIED.,.F.,.F.,(4,1,1,1,4),(40.8407044966673,41.1097812328693,
42.084928565179,43.0600758974886,44.0352232297983),.UNSPECIFIED.);
#528=B_SPLINE_CURVE_WITH_KNOTS('',3,(#18868,#18869,#18870,#18871,#18872,
#18873,#18874),.UNSPECIFIED.,.F.,.F.,(4,1,1,1,4),(40.8407044966673,41.7025254316425,
42.6776727639522,43.6528200962618,44.5576896014339),.UNSPECIFIED.);
#529=B_SPLINE_CURVE_WITH_KNOTS('',3,(#18879,#18880,#18881,#18882,#18883,
#18884,#18885,#18886,#18887,#18888),.UNSPECIFIED.,.F.,.F.,(4,1,1,1,1,1,
1,4),(34.5575191894877,35.2588972390113,36.234044571321,37.2091919036307,
38.1843392359403,39.15948656825,40.1346339005596,40.8407044966673),
 .UNSPECIFIED.);
#530=B_SPLINE_CURVE_WITH_KNOTS('',3,(#18889,#18890,#18891,#18892,#18893,
#18894,#18895,#18896,#18897,#18898,#18899),.UNSPECIFIED.,.F.,.F.,(4,1,1,
1,1,1,1,1,4),(34.5575191894877,34.8764941054748,35.8516414377845,36.8267887700942,
37.8019361024038,38.7770834347135,39.7522307670232,40.7273780993328,40.8407044966673),
 .UNSPECIFIED.);
#531=B_SPLINE_CURVE_WITH_KNOTS('',3,(#18904,#18905,#18906,#18907,#18908,
#18909,#18910,#18911,#18912,#18913,#18914),.UNSPECIFIED.,.F.,.F.,(4,1,1,
1,1,1,1,1,4),(28.2743338823081,28.4328659128437,29.4080132451533,30.383160577463,
31.3583079097727,32.3334552420823,33.308602574392,34.2837499067017,34.5575191894877),
 .UNSPECIFIED.);
#532=B_SPLINE_CURVE_WITH_KNOTS('',3,(#18915,#18916,#18917,#18918,#18919,
#18920,#18921,#18922,#18923,#18924),.UNSPECIFIED.,.F.,.F.,(4,1,1,1,1,1,
1,4),(28.2743338823081,29.0256101116168,30.0007574439265,30.9759047762362,
31.9510521085458,32.9261994408555,33.9013467731652,34.5575191894877),
 .UNSPECIFIED.);
#533=B_SPLINE_CURVE_WITH_KNOTS('',3,(#18929,#18930,#18931,#18932,#18933,
#18934,#18935,#18936,#18937,#18938),.UNSPECIFIED.,.F.,.F.,(4,1,1,1,1,1,
1,4),(21.9911485751285,22.5819819189857,23.5571292512954,24.532276583605,
25.5074239159147,26.4825712482243,27.457718580534,28.2743338823081),
 .UNSPECIFIED.);
#534=B_SPLINE_CURVE_WITH_KNOTS('',3,(#18939,#18940,#18941,#18942,#18943,
#18944,#18945,#18946,#18947,#18948,#18949),.UNSPECIFIED.,.F.,.F.,(4,1,1,
1,1,1,1,1,4),(21.9911485751285,22.1995787854492,23.1747261177589,24.1498734500685,
25.1250207823782,26.1001681146879,27.0753154469975,28.0504627793072,28.2743338823081),
 .UNSPECIFIED.);
#535=B_SPLINE_CURVE_WITH_KNOTS('',3,(#18955,#18956,#18957,#18958,#18959),
 .UNSPECIFIED.,.F.,.F.,(4,1,4),(14.3984001269719,15.3735474592815,15.7079632679489),
 .UNSPECIFIED.);
#536=B_SPLINE_CURVE_WITH_KNOTS('',3,(#18962,#18963,#18964,#18965,#18966),
 .UNSPECIFIED.,.F.,.F.,(4,1,4),(13.8759337553363,14.7808032605084,15.7079632679489),
 .UNSPECIFIED.);
#537=B_SPLINE_CURVE_WITH_KNOTS('',3,(#18968,#18969,#18970,#18971,#18972,
#18973,#18974,#18975,#18976,#18977,#18978),.UNSPECIFIED.,.F.,.F.,(4,1,1,
1,1,1,1,1,4),(15.7079632679489,15.755950592818,16.7310979251277,17.7062452574374,
18.681392589747,19.6565399220567,20.6316872543664,21.606834586676,21.9911485751285),
 .UNSPECIFIED.);
#538=B_SPLINE_CURVE_WITH_KNOTS('',3,(#18979,#18980,#18981,#18982,#18983,
#18984,#18985,#18986,#18987,#18988),.UNSPECIFIED.,.F.,.F.,(4,1,1,1,1,1,
1,4),(15.7079632679489,16.3486947915912,17.3238421239009,18.2989894562105,
19.2741367885202,20.2492841208299,21.2244314531395,21.9911485751285),
 .UNSPECIFIED.);
#539=B_SPLINE_CURVE_WITH_KNOTS('',3,(#19133,#19134,#19135,#19136,#19137,
#19138,#19139,#19140,#19141,#19142,#19143,#19144,#19145,#19146,#19147,#19148,
#19149,#19150,#19151,#19152,#19153,#19154,#19155,#19156,#19157,#19158,#19159,
#19160,#19161,#19162,#19163,#19164,#19165,#19166,#19167,#19168,#19169,#19170,
#19171,#19172,#19173,#19174,#19175,#19176,#19177,#19178,#19179,#19180,#19181),
 .UNSPECIFIED.,.F.,.F.,(4,3,3,3,3,3,3,3,3,3,3,3,3,3,3,3,4),(0.,0.0320333804888866,
0.0505515708593653,0.0603413132804416,0.0917900141854983,0.108096115778005,
0.122914675479851,0.145143248337739,0.168151513577436,0.177516949333476,
0.202471322707608,0.21794283081622,0.231200110368267,0.247503117401854,
0.263651632124391,0.277334442830003,0.286347380332244),.UNSPECIFIED.);
#540=B_SPLINE_CURVE_WITH_KNOTS('',3,(#19182,#19183,#19184,#19185,#19186,
#19187,#19188,#19189,#19190,#19191,#19192,#19193,#19194,#19195,#19196,#19197,
#19198,#19199,#19200,#19201,#19202,#19203,#19204,#19205,#19206,#19207,#19208,
#19209,#19210,#19211,#19212,#19213,#19214,#19215,#19216,#19217,#19218,#19219,
#19220,#19221,#19222,#19223,#19224,#19225,#19226,#19227,#19228,#19229,#19230),
 .UNSPECIFIED.,.F.,.F.,(4,3,3,3,3,3,3,3,3,3,3,3,3,3,3,3,4),(0.,0.0274305464075637,
0.0492901149097146,0.0591933555873536,0.0887250095166089,0.100015570674795,
0.108381796308415,0.130826479038955,0.152531076563578,0.162815893631175,
0.190691958353668,0.212372986031639,0.222945305605857,0.245534254906135,
0.257847836118801,0.274320152521146,0.28514280399515),.UNSPECIFIED.);
#541=B_SPLINE_CURVE_WITH_KNOTS('',3,(#19231,#19232,#19233,#19234,#19235,
#19236,#19237,#19238,#19239,#19240,#19241,#19242,#19243,#19244,#19245,#19246,
#19247,#19248,#19249,#19250,#19251,#19252,#19253,#19254,#19255),
 .UNSPECIFIED.,.F.,.F.,(4,3,3,3,3,3,3,3,4),(-10.1357873115492,-9.75147332309665,
-8.77632599078699,-7.80117865847732,-6.82603132616766,-5.85088399385799,
-4.87573666154833,-3.90058932923866,-3.8526020043696),.UNSPECIFIED.);
#542=B_SPLINE_CURVE_WITH_KNOTS('',3,(#19400,#19401,#19402,#19403,#19404,
#19405,#19406,#19407,#19408,#19409,#19410,#19411,#19412,#19413,#19414,#19415,
#19416,#19417,#19418,#19419,#19420,#19421,#19422,#19423,#19424,#19425,#19426,
#19427,#19428,#19429,#19430,#19431,#19432,#19433,#19434,#19435,#19436,#19437,
#19438,#19439,#19440,#19441,#19442,#19443,#19444,#19445,#19446,#19447,#19448),
 .UNSPECIFIED.,.F.,.F.,(4,3,3,3,3,3,3,3,3,3,3,3,3,3,3,3,4),(0.,0.0274305890506951,
0.0492901290331875,0.0591933603491513,0.0887250177779717,0.100015607166709,
0.108381835831352,0.13082647903896,0.152531071764912,0.162815892251191,
0.190691957318683,0.212372984486691,0.22294529735758,0.245534140364172,
0.257847701250626,0.274320152521159,0.285142803995162),.UNSPECIFIED.);
#543=B_SPLINE_CURVE_WITH_KNOTS('',3,(#19449,#19450,#19451,#19452,#19453,
#19454,#19455,#19456,#19457,#19458,#19459,#19460,#19461,#19462,#19463,#19464,
#19465,#19466,#19467,#19468,#19469,#19470,#19471,#19472,#19473),
 .UNSPECIFIED.,.F.,.F.,(4,3,3,3,3,3,3,3,4),(7.59274844815668,7.80117865847732,
8.77632599078698,9.75147332309665,10.7266206554063,11.701767987716,12.6769153200256,
13.6520626523353,13.8759337553363),.UNSPECIFIED.);
#544=B_SPLINE_CURVE_WITH_KNOTS('',3,(#19474,#19475,#19476,#19477,#19478,
#19479,#19480,#19481,#19482,#19483,#19484,#19485,#19486,#19487,#19488,#19489,
#19490,#19491,#19492,#19493,#19494,#19495,#19496,#19497,#19498,#19499,#19500,
#19501,#19502,#19503,#19504,#19505,#19506,#19507,#19508,#19509,#19510,#19511,
#19512,#19513,#19514,#19515,#19516,#19517,#19518,#19519,#19520,#19521,#19522),
 .UNSPECIFIED.,.F.,.F.,(4,3,3,3,3,3,3,3,3,3,3,3,3,3,3,3,4),(0.,0.0320334058164849,
0.0505515938322513,0.0603413311462071,0.0917900214840119,0.108096111687201,
0.122914678304232,0.145143248337743,0.168151527562726,0.177516955081398,
0.202471327018552,0.217942288122009,0.231200024743484,0.24750284136614,
0.263651600306541,0.277334442830014,0.286347380332252),.UNSPECIFIED.);
#545=SHAPE_REPRESENTATION_RELATIONSHIP('SRR','None',#19664,#555);
#546=SHAPE_REPRESENTATION_RELATIONSHIP('SRR','None',#19665,#556);
#547=SHAPE_REPRESENTATION_RELATIONSHIP('SRR','None',#19666,#557);
#548=SHAPE_REPRESENTATION_RELATIONSHIP('SRR','None',#19667,#558);
#549=SHAPE_REPRESENTATION_RELATIONSHIP('SRR','None',#19669,#559);
#550=SHAPE_REPRESENTATION_RELATIONSHIP('SRR','None',#19670,#560);
#551=SHAPE_REPRESENTATION_RELATIONSHIP('SRR','None',#19671,#561);
#552=SHAPE_REPRESENTATION_RELATIONSHIP('SRR','None',#19672,#562);
#553=SHAPE_REPRESENTATION_RELATIONSHIP('SRR','None',#19673,#563);
#554=SHAPE_REPRESENTATION_RELATIONSHIP('SRR','None',#19674,#564);
#555=ADVANCED_BREP_SHAPE_REPRESENTATION('',(#575),#19607);
#556=ADVANCED_BREP_SHAPE_REPRESENTATION('',(#576),#19608);
#557=ADVANCED_BREP_SHAPE_REPRESENTATION('',(#577),#19609);
#558=ADVANCED_BREP_SHAPE_REPRESENTATION('',(#578),#19610);
#559=ADVANCED_BREP_SHAPE_REPRESENTATION('',(#579),#19612);
#560=ADVANCED_BREP_SHAPE_REPRESENTATION('',(#580),#19613);
#561=ADVANCED_BREP_SHAPE_REPRESENTATION('',(#581),#19614);
#562=ADVANCED_BREP_SHAPE_REPRESENTATION('',(#582),#19615);
#563=ADVANCED_BREP_SHAPE_REPRESENTATION('',(#583),#19616);
#564=ADVANCED_BREP_SHAPE_REPRESENTATION('',(#584),#19617);
#565=STYLED_ITEM('',(#19728),#575);
#566=STYLED_ITEM('',(#19728),#576);
#567=STYLED_ITEM('',(#19729),#577);
#568=STYLED_ITEM('',(#19730),#578);
#569=STYLED_ITEM('',(#19731),#579);
#570=STYLED_ITEM('',(#19731),#580);
#571=STYLED_ITEM('',(#19732),#581);
#572=STYLED_ITEM('',(#19730),#582);
#573=STYLED_ITEM('',(#19733),#583);
#574=STYLED_ITEM('',(#19734),#584);
#575=MANIFOLD_SOLID_BREP('Body1',#7103);
#576=MANIFOLD_SOLID_BREP('Body1',#7104);
#577=MANIFOLD_SOLID_BREP('Body1',#7105);
#578=MANIFOLD_SOLID_BREP('Body1',#7106);
#579=MANIFOLD_SOLID_BREP('Body1',#7107);
#580=MANIFOLD_SOLID_BREP('Body1',#7108);
#581=MANIFOLD_SOLID_BREP('Body1',#7109);
#582=MANIFOLD_SOLID_BREP('Body1',#7110);
#583=MANIFOLD_SOLID_BREP('Body1',#7111);
#584=MANIFOLD_SOLID_BREP('Body1',#7112);
#585=TOROIDAL_SURFACE('',#7263,1.2,0.1);
#586=TOROIDAL_SURFACE('',#7273,1.2,0.1);
#587=TOROIDAL_SURFACE('',#7321,1.2,0.1);
#588=TOROIDAL_SURFACE('',#7331,1.2,0.1);
#589=FACE_BOUND('',#1242,.T.);
#590=FACE_BOUND('',#1243,.T.);
#591=FACE_BOUND('',#1244,.T.);
#592=FACE_BOUND('',#1245,.T.);
#593=FACE_BOUND('',#1249,.T.);
#594=FACE_BOUND('',#1250,.T.);
#595=FACE_BOUND('',#1251,.T.);
#596=FACE_BOUND('',#1252,.T.);
#597=FACE_BOUND('',#1280,.T.);
#598=FACE_BOUND('',#1281,.T.);
#599=FACE_BOUND('',#1282,.T.);
#600=FACE_BOUND('',#1283,.T.);
#601=FACE_BOUND('',#1287,.T.);
#602=FACE_BOUND('',#1288,.T.);
#603=FACE_BOUND('',#1289,.T.);
#604=FACE_BOUND('',#1290,.T.);
#605=FACE_BOUND('',#1304,.T.);
#606=FACE_BOUND('',#1306,.T.);
#607=FACE_BOUND('',#1309,.T.);
#608=FACE_BOUND('',#1321,.T.);
#609=FACE_BOUND('',#1322,.T.);
#610=FACE_BOUND('',#1323,.T.);
#611=FACE_BOUND('',#1330,.T.);
#612=FACE_BOUND('',#1333,.T.);
#613=FACE_BOUND('',#1344,.T.);
#614=FACE_BOUND('',#1346,.T.);
#615=FACE_BOUND('',#1358,.T.);
#616=FACE_BOUND('',#1367,.T.);
#617=FACE_BOUND('',#1368,.T.);
#618=FACE_BOUND('',#1369,.T.);
#619=FACE_BOUND('',#1418,.T.);
#620=FACE_BOUND('',#1419,.T.);
#621=FACE_BOUND('',#1420,.T.);
#622=FACE_BOUND('',#1421,.T.);
#623=FACE_BOUND('',#1422,.T.);
#624=FACE_BOUND('',#1423,.T.);
#625=FACE_BOUND('',#1427,.T.);
#626=FACE_BOUND('',#1428,.T.);
#627=FACE_BOUND('',#1429,.T.);
#628=FACE_BOUND('',#1441,.T.);
#629=FACE_BOUND('',#1449,.T.);
#630=FACE_BOUND('',#1460,.T.);
#631=FACE_BOUND('',#1462,.T.);
#632=FACE_BOUND('',#1474,.T.);
#633=FACE_BOUND('',#1483,.T.);
#634=FACE_BOUND('',#1484,.T.);
#635=FACE_BOUND('',#1485,.T.);
#636=FACE_BOUND('',#1534,.T.);
#637=FACE_BOUND('',#1535,.T.);
#638=FACE_BOUND('',#1536,.T.);
#639=FACE_BOUND('',#1537,.T.);
#640=FACE_BOUND('',#1538,.T.);
#641=FACE_BOUND('',#1539,.T.);
#642=FACE_BOUND('',#1545,.T.);
#643=FACE_BOUND('',#1549,.T.);
#644=FACE_BOUND('',#1553,.T.);
#645=FACE_BOUND('',#1557,.T.);
#646=FACE_BOUND('',#1577,.T.);
#647=FACE_BOUND('',#1578,.T.);
#648=FACE_BOUND('',#1583,.T.);
#649=FACE_BOUND('',#1584,.T.);
#650=FACE_BOUND('',#1585,.T.);
#651=FACE_BOUND('',#1586,.T.);
#652=FACE_BOUND('',#1587,.T.);
#653=FACE_BOUND('',#1588,.T.);
#654=FACE_BOUND('',#1663,.T.);
#655=FACE_BOUND('',#1666,.T.);
#656=FACE_BOUND('',#1682,.T.);
#657=FACE_BOUND('',#1691,.T.);
#658=FACE_BOUND('',#1695,.T.);
#659=FACE_BOUND('',#1697,.T.);
#660=CONICAL_SURFACE('',#7236,3.28832599394285,0.927295218001612);
#661=CONICAL_SURFACE('',#7699,0.1,0.785398163397448);
#662=PLANE('',#7235);
#663=PLANE('',#7239);
#664=PLANE('',#7240);
#665=PLANE('',#7241);
#666=PLANE('',#7248);
#667=PLANE('',#7249);
#668=PLANE('',#7250);
#669=PLANE('',#7251);
#670=PLANE('',#7252);
#671=PLANE('',#7259);
#672=PLANE('',#7270);
#673=PLANE('',#7277);
#674=PLANE('',#7278);
#675=PLANE('',#7279);
#676=PLANE('',#7280);
#677=PLANE('',#7281);
#678=PLANE('',#7282);
#679=PLANE('',#7283);
#680=PLANE('',#7284);
#681=PLANE('',#7295);
#682=PLANE('',#7296);
#683=PLANE('',#7306);
#684=PLANE('',#7307);
#685=PLANE('',#7308);
#686=PLANE('',#7309);
#687=PLANE('',#7310);
#688=PLANE('',#7317);
#689=PLANE('',#7328);
#690=PLANE('',#7335);
#691=PLANE('',#7336);
#692=PLANE('',#7337);
#693=PLANE('',#7338);
#694=PLANE('',#7339);
#695=PLANE('',#7340);
#696=PLANE('',#7341);
#697=PLANE('',#7342);
#698=PLANE('',#7347);
#699=PLANE('',#7349);
#700=PLANE('',#7353);
#701=PLANE('',#7358);
#702=PLANE('',#7360);
#703=PLANE('',#7362);
#704=PLANE('',#7363);
#705=PLANE('',#7364);
#706=PLANE('',#7371);
#707=PLANE('',#7374);
#708=PLANE('',#7391);
#709=PLANE('',#7396);
#710=PLANE('',#7402);
#711=PLANE('',#7403);
#712=PLANE('',#7404);
#713=PLANE('',#7405);
#714=PLANE('',#7406);
#715=PLANE('',#7407);
#716=PLANE('',#7408);
#717=PLANE('',#7409);
#718=PLANE('',#7411);
#719=PLANE('',#7413);
#720=PLANE('',#7414);
#721=PLANE('',#7415);
#722=PLANE('',#7416);
#723=PLANE('',#7417);
#724=PLANE('',#7418);
#725=PLANE('',#7419);
#726=PLANE('',#7420);
#727=PLANE('',#7421);
#728=PLANE('',#7422);
#729=PLANE('',#7423);
#730=PLANE('',#7427);
#731=PLANE('',#7429);
#732=PLANE('',#7430);
#733=PLANE('',#7431);
#734=PLANE('',#7432);
#735=PLANE('',#7433);
#736=PLANE('',#7434);
#737=PLANE('',#7436);
#738=PLANE('',#7453);
#739=PLANE('',#7472);
#740=PLANE('',#7473);
#741=PLANE('',#7474);
#742=PLANE('',#7476);
#743=PLANE('',#7490);
#744=PLANE('',#7491);
#745=PLANE('',#7492);
#746=PLANE('',#7493);
#747=PLANE('',#7494);
#748=PLANE('',#7495);
#749=PLANE('',#7496);
#750=PLANE('',#7498);
#751=PLANE('',#7499);
#752=PLANE('',#7500);
#753=PLANE('',#7501);
#754=PLANE('',#7502);
#755=PLANE('',#7503);
#756=PLANE('',#7504);
#757=PLANE('',#7510);
#758=PLANE('',#7511);
#759=PLANE('',#7512);
#760=PLANE('',#7513);
#761=PLANE('',#7514);
#762=PLANE('',#7515);
#763=PLANE('',#7516);
#764=PLANE('',#7517);
#765=PLANE('',#7519);
#766=PLANE('',#7521);
#767=PLANE('',#7522);
#768=PLANE('',#7523);
#769=PLANE('',#7524);
#770=PLANE('',#7525);
#771=PLANE('',#7526);
#772=PLANE('',#7527);
#773=PLANE('',#7528);
#774=PLANE('',#7529);
#775=PLANE('',#7530);
#776=PLANE('',#7531);
#777=PLANE('',#7535);
#778=PLANE('',#7537);
#779=PLANE('',#7538);
#780=PLANE('',#7539);
#781=PLANE('',#7540);
#782=PLANE('',#7541);
#783=PLANE('',#7542);
#784=PLANE('',#7544);
#785=PLANE('',#7561);
#786=PLANE('',#7580);
#787=PLANE('',#7581);
#788=PLANE('',#7582);
#789=PLANE('',#7590);
#790=PLANE('',#7595);
#791=PLANE('',#7596);
#792=PLANE('',#7601);
#793=PLANE('',#7602);
#794=PLANE('',#7607);
#795=PLANE('',#7608);
#796=PLANE('',#7613);
#797=PLANE('',#7632);
#798=PLANE('',#7633);
#799=PLANE('',#7634);
#800=PLANE('',#7635);
#801=PLANE('',#7705);
#802=PLANE('',#7706);
#803=PLANE('',#7707);
#804=PLANE('',#7708);
#805=PLANE('',#7709);
#806=PLANE('',#7710);
#807=PLANE('',#7711);
#808=PLANE('',#7712);
#809=PLANE('',#7716);
#810=PLANE('',#7717);
#811=PLANE('',#7735);
#812=PLANE('',#7737);
#813=PLANE('',#7738);
#814=PLANE('',#7739);
#815=PLANE('',#7740);
#816=PLANE('',#7741);
#817=PLANE('',#7742);
#818=PLANE('',#7743);
#819=PLANE('',#7759);
#820=PLANE('',#7760);
#821=FACE_OUTER_BOUND('',#1224,.T.);
#822=FACE_OUTER_BOUND('',#1225,.T.);
#823=FACE_OUTER_BOUND('',#1226,.T.);
#824=FACE_OUTER_BOUND('',#1227,.T.);
#825=FACE_OUTER_BOUND('',#1228,.T.);
#826=FACE_OUTER_BOUND('',#1229,.T.);
#827=FACE_OUTER_BOUND('',#1230,.T.);
#828=FACE_OUTER_BOUND('',#1231,.T.);
#829=FACE_OUTER_BOUND('',#1232,.T.);
#830=FACE_OUTER_BOUND('',#1233,.T.);
#831=FACE_OUTER_BOUND('',#1234,.T.);
#832=FACE_OUTER_BOUND('',#1235,.T.);
#833=FACE_OUTER_BOUND('',#1236,.T.);
#834=FACE_OUTER_BOUND('',#1237,.T.);
#835=FACE_OUTER_BOUND('',#1238,.T.);
#836=FACE_OUTER_BOUND('',#1239,.T.);
#837=FACE_OUTER_BOUND('',#1240,.T.);
#838=FACE_OUTER_BOUND('',#1241,.T.);
#839=FACE_OUTER_BOUND('',#1246,.T.);
#840=FACE_OUTER_BOUND('',#1247,.T.);
#841=FACE_OUTER_BOUND('',#1248,.T.);
#842=FACE_OUTER_BOUND('',#1253,.T.);
#843=FACE_OUTER_BOUND('',#1254,.T.);
#844=FACE_OUTER_BOUND('',#1255,.T.);
#845=FACE_OUTER_BOUND('',#1256,.T.);
#846=FACE_OUTER_BOUND('',#1257,.T.);
#847=FACE_OUTER_BOUND('',#1258,.T.);
#848=FACE_OUTER_BOUND('',#1259,.T.);
#849=FACE_OUTER_BOUND('',#1260,.T.);
#850=FACE_OUTER_BOUND('',#1261,.T.);
#851=FACE_OUTER_BOUND('',#1262,.T.);
#852=FACE_OUTER_BOUND('',#1263,.T.);
#853=FACE_OUTER_BOUND('',#1264,.T.);
#854=FACE_OUTER_BOUND('',#1265,.T.);
#855=FACE_OUTER_BOUND('',#1266,.T.);
#856=FACE_OUTER_BOUND('',#1267,.T.);
#857=FACE_OUTER_BOUND('',#1268,.T.);
#858=FACE_OUTER_BOUND('',#1269,.T.);
#859=FACE_OUTER_BOUND('',#1270,.T.);
#860=FACE_OUTER_BOUND('',#1271,.T.);
#861=FACE_OUTER_BOUND('',#1272,.T.);
#862=FACE_OUTER_BOUND('',#1273,.T.);
#863=FACE_OUTER_BOUND('',#1274,.T.);
#864=FACE_OUTER_BOUND('',#1275,.T.);
#865=FACE_OUTER_BOUND('',#1276,.T.);
#866=FACE_OUTER_BOUND('',#1277,.T.);
#867=FACE_OUTER_BOUND('',#1278,.T.);
#868=FACE_OUTER_BOUND('',#1279,.T.);
#869=FACE_OUTER_BOUND('',#1284,.T.);
#870=FACE_OUTER_BOUND('',#1285,.T.);
#871=FACE_OUTER_BOUND('',#1286,.T.);
#872=FACE_OUTER_BOUND('',#1291,.T.);
#873=FACE_OUTER_BOUND('',#1292,.T.);
#874=FACE_OUTER_BOUND('',#1293,.T.);
#875=FACE_OUTER_BOUND('',#1294,.T.);
#876=FACE_OUTER_BOUND('',#1295,.T.);
#877=FACE_OUTER_BOUND('',#1296,.T.);
#878=FACE_OUTER_BOUND('',#1297,.T.);
#879=FACE_OUTER_BOUND('',#1298,.T.);
#880=FACE_OUTER_BOUND('',#1299,.T.);
#881=FACE_OUTER_BOUND('',#1300,.T.);
#882=FACE_OUTER_BOUND('',#1301,.T.);
#883=FACE_OUTER_BOUND('',#1302,.T.);
#884=FACE_OUTER_BOUND('',#1303,.T.);
#885=FACE_OUTER_BOUND('',#1305,.T.);
#886=FACE_OUTER_BOUND('',#1307,.T.);
#887=FACE_OUTER_BOUND('',#1308,.T.);
#888=FACE_OUTER_BOUND('',#1310,.T.);
#889=FACE_OUTER_BOUND('',#1311,.T.);
#890=FACE_OUTER_BOUND('',#1312,.T.);
#891=FACE_OUTER_BOUND('',#1313,.T.);
#892=FACE_OUTER_BOUND('',#1314,.T.);
#893=FACE_OUTER_BOUND('',#1315,.T.);
#894=FACE_OUTER_BOUND('',#1316,.T.);
#895=FACE_OUTER_BOUND('',#1317,.T.);
#896=FACE_OUTER_BOUND('',#1318,.T.);
#897=FACE_OUTER_BOUND('',#1319,.T.);
#898=FACE_OUTER_BOUND('',#1320,.T.);
#899=FACE_OUTER_BOUND('',#1324,.T.);
#900=FACE_OUTER_BOUND('',#1325,.T.);
#901=FACE_OUTER_BOUND('',#1326,.T.);
#902=FACE_OUTER_BOUND('',#1327,.T.);
#903=FACE_OUTER_BOUND('',#1328,.T.);
#904=FACE_OUTER_BOUND('',#1329,.T.);
#905=FACE_OUTER_BOUND('',#1331,.T.);
#906=FACE_OUTER_BOUND('',#1332,.T.);
#907=FACE_OUTER_BOUND('',#1334,.T.);
#908=FACE_OUTER_BOUND('',#1335,.T.);
#909=FACE_OUTER_BOUND('',#1336,.T.);
#910=FACE_OUTER_BOUND('',#1337,.T.);
#911=FACE_OUTER_BOUND('',#1338,.T.);
#912=FACE_OUTER_BOUND('',#1339,.T.);
#913=FACE_OUTER_BOUND('',#1340,.T.);
#914=FACE_OUTER_BOUND('',#1341,.T.);
#915=FACE_OUTER_BOUND('',#1342,.T.);
#916=FACE_OUTER_BOUND('',#1343,.T.);
#917=FACE_OUTER_BOUND('',#1345,.T.);
#918=FACE_OUTER_BOUND('',#1347,.T.);
#919=FACE_OUTER_BOUND('',#1348,.T.);
#920=FACE_OUTER_BOUND('',#1349,.T.);
#921=FACE_OUTER_BOUND('',#1350,.T.);
#922=FACE_OUTER_BOUND('',#1351,.T.);
#923=FACE_OUTER_BOUND('',#1352,.T.);
#924=FACE_OUTER_BOUND('',#1353,.T.);
#925=FACE_OUTER_BOUND('',#1354,.T.);
#926=FACE_OUTER_BOUND('',#1355,.T.);
#927=FACE_OUTER_BOUND('',#1356,.T.);
#928=FACE_OUTER_BOUND('',#1357,.T.);
#929=FACE_OUTER_BOUND('',#1359,.T.);
#930=FACE_OUTER_BOUND('',#1360,.T.);
#931=FACE_OUTER_BOUND('',#1361,.T.);
#932=FACE_OUTER_BOUND('',#1362,.T.);
#933=FACE_OUTER_BOUND('',#1363,.T.);
#934=FACE_OUTER_BOUND('',#1364,.T.);
#935=FACE_OUTER_BOUND('',#1365,.T.);
#936=FACE_OUTER_BOUND('',#1366,.T.);
#937=FACE_OUTER_BOUND('',#1370,.T.);
#938=FACE_OUTER_BOUND('',#1371,.T.);
#939=FACE_OUTER_BOUND('',#1372,.T.);
#940=FACE_OUTER_BOUND('',#1373,.T.);
#941=FACE_OUTER_BOUND('',#1374,.T.);
#942=FACE_OUTER_BOUND('',#1375,.T.);
#943=FACE_OUTER_BOUND('',#1376,.T.);
#944=FACE_OUTER_BOUND('',#1377,.T.);
#945=FACE_OUTER_BOUND('',#1378,.T.);
#946=FACE_OUTER_BOUND('',#1379,.T.);
#947=FACE_OUTER_BOUND('',#1380,.T.);
#948=FACE_OUTER_BOUND('',#1381,.T.);
#949=FACE_OUTER_BOUND('',#1382,.T.);
#950=FACE_OUTER_BOUND('',#1383,.T.);
#951=FACE_OUTER_BOUND('',#1384,.T.);
#952=FACE_OUTER_BOUND('',#1385,.T.);
#953=FACE_OUTER_BOUND('',#1386,.T.);
#954=FACE_OUTER_BOUND('',#1387,.T.);
#955=FACE_OUTER_BOUND('',#1388,.T.);
#956=FACE_OUTER_BOUND('',#1389,.T.);
#957=FACE_OUTER_BOUND('',#1390,.T.);
#958=FACE_OUTER_BOUND('',#1391,.T.);
#959=FACE_OUTER_BOUND('',#1392,.T.);
#960=FACE_OUTER_BOUND('',#1393,.T.);
#961=FACE_OUTER_BOUND('',#1394,.T.);
#962=FACE_OUTER_BOUND('',#1395,.T.);
#963=FACE_OUTER_BOUND('',#1396,.T.);
#964=FACE_OUTER_BOUND('',#1397,.T.);
#965=FACE_OUTER_BOUND('',#1398,.T.);
#966=FACE_OUTER_BOUND('',#1399,.T.);
#967=FACE_OUTER_BOUND('',#1400,.T.);
#968=FACE_OUTER_BOUND('',#1401,.T.);
#969=FACE_OUTER_BOUND('',#1402,.T.);
#970=FACE_OUTER_BOUND('',#1403,.T.);
#971=FACE_OUTER_BOUND('',#1404,.T.);
#972=FACE_OUTER_BOUND('',#1405,.T.);
#973=FACE_OUTER_BOUND('',#1406,.T.);
#974=FACE_OUTER_BOUND('',#1407,.T.);
#975=FACE_OUTER_BOUND('',#1408,.T.);
#976=FACE_OUTER_BOUND('',#1409,.T.);
#977=FACE_OUTER_BOUND('',#1410,.T.);
#978=FACE_OUTER_BOUND('',#1411,.T.);
#979=FACE_OUTER_BOUND('',#1412,.T.);
#980=FACE_OUTER_BOUND('',#1413,.T.);
#981=FACE_OUTER_BOUND('',#1414,.T.);
#982=FACE_OUTER_BOUND('',#1415,.T.);
#983=FACE_OUTER_BOUND('',#1416,.T.);
#984=FACE_OUTER_BOUND('',#1417,.T.);
#985=FACE_OUTER_BOUND('',#1424,.T.);
#986=FACE_OUTER_BOUND('',#1425,.T.);
#987=FACE_OUTER_BOUND('',#1426,.T.);
#988=FACE_OUTER_BOUND('',#1430,.T.);
#989=FACE_OUTER_BOUND('',#1431,.T.);
#990=FACE_OUTER_BOUND('',#1432,.T.);
#991=FACE_OUTER_BOUND('',#1433,.T.);
#992=FACE_OUTER_BOUND('',#1434,.T.);
#993=FACE_OUTER_BOUND('',#1435,.T.);
#994=FACE_OUTER_BOUND('',#1436,.T.);
#995=FACE_OUTER_BOUND('',#1437,.T.);
#996=FACE_OUTER_BOUND('',#1438,.T.);
#997=FACE_OUTER_BOUND('',#1439,.T.);
#998=FACE_OUTER_BOUND('',#1440,.T.);
#999=FACE_OUTER_BOUND('',#1442,.T.);
#1000=FACE_OUTER_BOUND('',#1443,.T.);
#1001=FACE_OUTER_BOUND('',#1444,.T.);
#1002=FACE_OUTER_BOUND('',#1445,.T.);
#1003=FACE_OUTER_BOUND('',#1446,.T.);
#1004=FACE_OUTER_BOUND('',#1447,.T.);
#1005=FACE_OUTER_BOUND('',#1448,.T.);
#1006=FACE_OUTER_BOUND('',#1450,.T.);
#1007=FACE_OUTER_BOUND('',#1451,.T.);
#1008=FACE_OUTER_BOUND('',#1452,.T.);
#1009=FACE_OUTER_BOUND('',#1453,.T.);
#1010=FACE_OUTER_BOUND('',#1454,.T.);
#1011=FACE_OUTER_BOUND('',#1455,.T.);
#1012=FACE_OUTER_BOUND('',#1456,.T.);
#1013=FACE_OUTER_BOUND('',#1457,.T.);
#1014=FACE_OUTER_BOUND('',#1458,.T.);
#1015=FACE_OUTER_BOUND('',#1459,.T.);
#1016=FACE_OUTER_BOUND('',#1461,.T.);
#1017=FACE_OUTER_BOUND('',#1463,.T.);
#1018=FACE_OUTER_BOUND('',#1464,.T.);
#1019=FACE_OUTER_BOUND('',#1465,.T.);
#1020=FACE_OUTER_BOUND('',#1466,.T.);
#1021=FACE_OUTER_BOUND('',#1467,.T.);
#1022=FACE_OUTER_BOUND('',#1468,.T.);
#1023=FACE_OUTER_BOUND('',#1469,.T.);
#1024=FACE_OUTER_BOUND('',#1470,.T.);
#1025=FACE_OUTER_BOUND('',#1471,.T.);
#1026=FACE_OUTER_BOUND('',#1472,.T.);
#1027=FACE_OUTER_BOUND('',#1473,.T.);
#1028=FACE_OUTER_BOUND('',#1475,.T.);
#1029=FACE_OUTER_BOUND('',#1476,.T.);
#1030=FACE_OUTER_BOUND('',#1477,.T.);
#1031=FACE_OUTER_BOUND('',#1478,.T.);
#1032=FACE_OUTER_BOUND('',#1479,.T.);
#1033=FACE_OUTER_BOUND('',#1480,.T.);
#1034=FACE_OUTER_BOUND('',#1481,.T.);
#1035=FACE_OUTER_BOUND('',#1482,.T.);
#1036=FACE_OUTER_BOUND('',#1486,.T.);
#1037=FACE_OUTER_BOUND('',#1487,.T.);
#1038=FACE_OUTER_BOUND('',#1488,.T.);
#1039=FACE_OUTER_BOUND('',#1489,.T.);
#1040=FACE_OUTER_BOUND('',#1490,.T.);
#1041=FACE_OUTER_BOUND('',#1491,.T.);
#1042=FACE_OUTER_BOUND('',#1492,.T.);
#1043=FACE_OUTER_BOUND('',#1493,.T.);
#1044=FACE_OUTER_BOUND('',#1494,.T.);
#1045=FACE_OUTER_BOUND('',#1495,.T.);
#1046=FACE_OUTER_BOUND('',#1496,.T.);
#1047=FACE_OUTER_BOUND('',#1497,.T.);
#1048=FACE_OUTER_BOUND('',#1498,.T.);
#1049=FACE_OUTER_BOUND('',#1499,.T.);
#1050=FACE_OUTER_BOUND('',#1500,.T.);
#1051=FACE_OUTER_BOUND('',#1501,.T.);
#1052=FACE_OUTER_BOUND('',#1502,.T.);
#1053=FACE_OUTER_BOUND('',#1503,.T.);
#1054=FACE_OUTER_BOUND('',#1504,.T.);
#1055=FACE_OUTER_BOUND('',#1505,.T.);
#1056=FACE_OUTER_BOUND('',#1506,.T.);
#1057=FACE_OUTER_BOUND('',#1507,.T.);
#1058=FACE_OUTER_BOUND('',#1508,.T.);
#1059=FACE_OUTER_BOUND('',#1509,.T.);
#1060=FACE_OUTER_BOUND('',#1510,.T.);
#1061=FACE_OUTER_BOUND('',#1511,.T.);
#1062=FACE_OUTER_BOUND('',#1512,.T.);
#1063=FACE_OUTER_BOUND('',#1513,.T.);
#1064=FACE_OUTER_BOUND('',#1514,.T.);
#1065=FACE_OUTER_BOUND('',#1515,.T.);
#1066=FACE_OUTER_BOUND('',#1516,.T.);
#1067=FACE_OUTER_BOUND('',#1517,.T.);
#1068=FACE_OUTER_BOUND('',#1518,.T.);
#1069=FACE_OUTER_BOUND('',#1519,.T.);
#1070=FACE_OUTER_BOUND('',#1520,.T.);
#1071=FACE_OUTER_BOUND('',#1521,.T.);
#1072=FACE_OUTER_BOUND('',#1522,.T.);
#1073=FACE_OUTER_BOUND('',#1523,.T.);
#1074=FACE_OUTER_BOUND('',#1524,.T.);
#1075=FACE_OUTER_BOUND('',#1525,.T.);
#1076=FACE_OUTER_BOUND('',#1526,.T.);
#1077=FACE_OUTER_BOUND('',#1527,.T.);
#1078=FACE_OUTER_BOUND('',#1528,.T.);
#1079=FACE_OUTER_BOUND('',#1529,.T.);
#1080=FACE_OUTER_BOUND('',#1530,.T.);
#1081=FACE_OUTER_BOUND('',#1531,.T.);
#1082=FACE_OUTER_BOUND('',#1532,.T.);
#1083=FACE_OUTER_BOUND('',#1533,.T.);
#1084=FACE_OUTER_BOUND('',#1540,.T.);
#1085=FACE_OUTER_BOUND('',#1541,.T.);
#1086=FACE_OUTER_BOUND('',#1542,.T.);
#1087=FACE_OUTER_BOUND('',#1543,.T.);
#1088=FACE_OUTER_BOUND('',#1544,.T.);
#1089=FACE_OUTER_BOUND('',#1546,.T.);
#1090=FACE_OUTER_BOUND('',#1547,.T.);
#1091=FACE_OUTER_BOUND('',#1548,.T.);
#1092=FACE_OUTER_BOUND('',#1550,.T.);
#1093=FACE_OUTER_BOUND('',#1551,.T.);
#1094=FACE_OUTER_BOUND('',#1552,.T.);
#1095=FACE_OUTER_BOUND('',#1554,.T.);
#1096=FACE_OUTER_BOUND('',#1555,.T.);
#1097=FACE_OUTER_BOUND('',#1556,.T.);
#1098=FACE_OUTER_BOUND('',#1558,.T.);
#1099=FACE_OUTER_BOUND('',#1559,.T.);
#1100=FACE_OUTER_BOUND('',#1560,.T.);
#1101=FACE_OUTER_BOUND('',#1561,.T.);
#1102=FACE_OUTER_BOUND('',#1562,.T.);
#1103=FACE_OUTER_BOUND('',#1563,.T.);
#1104=FACE_OUTER_BOUND('',#1564,.T.);
#1105=FACE_OUTER_BOUND('',#1565,.T.);
#1106=FACE_OUTER_BOUND('',#1566,.T.);
#1107=FACE_OUTER_BOUND('',#1567,.T.);
#1108=FACE_OUTER_BOUND('',#1568,.T.);
#1109=FACE_OUTER_BOUND('',#1569,.T.);
#1110=FACE_OUTER_BOUND('',#1570,.T.);
#1111=FACE_OUTER_BOUND('',#1571,.T.);
#1112=FACE_OUTER_BOUND('',#1572,.T.);
#1113=FACE_OUTER_BOUND('',#1573,.T.);
#1114=FACE_OUTER_BOUND('',#1574,.T.);
#1115=FACE_OUTER_BOUND('',#1575,.T.);
#1116=FACE_OUTER_BOUND('',#1576,.T.);
#1117=FACE_OUTER_BOUND('',#1579,.T.);
#1118=FACE_OUTER_BOUND('',#1580,.T.);
#1119=FACE_OUTER_BOUND('',#1581,.T.);
#1120=FACE_OUTER_BOUND('',#1582,.T.);
#1121=FACE_OUTER_BOUND('',#1589,.T.);
#1122=FACE_OUTER_BOUND('',#1590,.T.);
#1123=FACE_OUTER_BOUND('',#1591,.T.);
#1124=FACE_OUTER_BOUND('',#1592,.T.);
#1125=FACE_OUTER_BOUND('',#1593,.T.);
#1126=FACE_OUTER_BOUND('',#1594,.T.);
#1127=FACE_OUTER_BOUND('',#1595,.T.);
#1128=FACE_OUTER_BOUND('',#1596,.T.);
#1129=FACE_OUTER_BOUND('',#1597,.T.);
#1130=FACE_OUTER_BOUND('',#1598,.T.);
#1131=FACE_OUTER_BOUND('',#1599,.T.);
#1132=FACE_OUTER_BOUND('',#1600,.T.);
#1133=FACE_OUTER_BOUND('',#1601,.T.);
#1134=FACE_OUTER_BOUND('',#1602,.T.);
#1135=FACE_OUTER_BOUND('',#1603,.T.);
#1136=FACE_OUTER_BOUND('',#1604,.T.);
#1137=FACE_OUTER_BOUND('',#1605,.T.);
#1138=FACE_OUTER_BOUND('',#1606,.T.);
#1139=FACE_OUTER_BOUND('',#1607,.T.);
#1140=FACE_OUTER_BOUND('',#1608,.T.);
#1141=FACE_OUTER_BOUND('',#1609,.T.);
#1142=FACE_OUTER_BOUND('',#1610,.T.);
#1143=FACE_OUTER_BOUND('',#1611,.T.);
#1144=FACE_OUTER_BOUND('',#1612,.T.);
#1145=FACE_OUTER_BOUND('',#1613,.T.);
#1146=FACE_OUTER_BOUND('',#1614,.T.);
#1147=FACE_OUTER_BOUND('',#1615,.T.);
#1148=FACE_OUTER_BOUND('',#1616,.T.);
#1149=FACE_OUTER_BOUND('',#1617,.T.);
#1150=FACE_OUTER_BOUND('',#1618,.T.);
#1151=FACE_OUTER_BOUND('',#1619,.T.);
#1152=FACE_OUTER_BOUND('',#1620,.T.);
#1153=FACE_OUTER_BOUND('',#1621,.T.);
#1154=FACE_OUTER_BOUND('',#1622,.T.);
#1155=FACE_OUTER_BOUND('',#1623,.T.);
#1156=FACE_OUTER_BOUND('',#1624,.T.);
#1157=FACE_OUTER_BOUND('',#1625,.T.);
#1158=FACE_OUTER_BOUND('',#1626,.T.);
#1159=FACE_OUTER_BOUND('',#1627,.T.);
#1160=FACE_OUTER_BOUND('',#1628,.T.);
#1161=FACE_OUTER_BOUND('',#1629,.T.);
#1162=FACE_OUTER_BOUND('',#1630,.T.);
#1163=FACE_OUTER_BOUND('',#1631,.T.);
#1164=FACE_OUTER_BOUND('',#1632,.T.);
#1165=FACE_OUTER_BOUND('',#1633,.T.);
#1166=FACE_OUTER_BOUND('',#1634,.T.);
#1167=FACE_OUTER_BOUND('',#1635,.T.);
#1168=FACE_OUTER_BOUND('',#1636,.T.);
#1169=FACE_OUTER_BOUND('',#1637,.T.);
#1170=FACE_OUTER_BOUND('',#1638,.T.);
#1171=FACE_OUTER_BOUND('',#1639,.T.);
#1172=FACE_OUTER_BOUND('',#1640,.T.);
#1173=FACE_OUTER_BOUND('',#1641,.T.);
#1174=FACE_OUTER_BOUND('',#1642,.T.);
#1175=FACE_OUTER_BOUND('',#1643,.T.);
#1176=FACE_OUTER_BOUND('',#1644,.T.);
#1177=FACE_OUTER_BOUND('',#1645,.T.);
#1178=FACE_OUTER_BOUND('',#1646,.T.);
#1179=FACE_OUTER_BOUND('',#1647,.T.);
#1180=FACE_OUTER_BOUND('',#1648,.T.);
#1181=FACE_OUTER_BOUND('',#1649,.T.);
#1182=FACE_OUTER_BOUND('',#1650,.T.);
#1183=FACE_OUTER_BOUND('',#1651,.T.);
#1184=FACE_OUTER_BOUND('',#1652,.T.);
#1185=FACE_OUTER_BOUND('',#1653,.T.);
#1186=FACE_OUTER_BOUND('',#1654,.T.);
#1187=FACE_OUTER_BOUND('',#1655,.T.);
#1188=FACE_OUTER_BOUND('',#1656,.T.);
#1189=FACE_OUTER_BOUND('',#1657,.T.);
#1190=FACE_OUTER_BOUND('',#1658,.T.);
#1191=FACE_OUTER_BOUND('',#1659,.T.);
#1192=FACE_OUTER_BOUND('',#1660,.T.);
#1193=FACE_OUTER_BOUND('',#1661,.T.);
#1194=FACE_OUTER_BOUND('',#1662,.T.);
#1195=FACE_OUTER_BOUND('',#1664,.T.);
#1196=FACE_OUTER_BOUND('',#1665,.T.);
#1197=FACE_OUTER_BOUND('',#1667,.T.);
#1198=FACE_OUTER_BOUND('',#1668,.T.);
#1199=FACE_OUTER_BOUND('',#1669,.T.);
#1200=FACE_OUTER_BOUND('',#1670,.T.);
#1201=FACE_OUTER_BOUND('',#1671,.T.);
#1202=FACE_OUTER_BOUND('',#1672,.T.);
#1203=FACE_OUTER_BOUND('',#1673,.T.);
#1204=FACE_OUTER_BOUND('',#1674,.T.);
#1205=FACE_OUTER_BOUND('',#1675,.T.);
#1206=FACE_OUTER_BOUND('',#1676,.T.);
#1207=FACE_OUTER_BOUND('',#1677,.T.);
#1208=FACE_OUTER_BOUND('',#1678,.T.);
#1209=FACE_OUTER_BOUND('',#1679,.T.);
#1210=FACE_OUTER_BOUND('',#1680,.T.);
#1211=FACE_OUTER_BOUND('',#1681,.T.);
#1212=FACE_OUTER_BOUND('',#1683,.T.);
#1213=FACE_OUTER_BOUND('',#1684,.T.);
#1214=FACE_OUTER_BOUND('',#1685,.T.);
#1215=FACE_OUTER_BOUND('',#1686,.T.);
#1216=FACE_OUTER_BOUND('',#1687,.T.);
#1217=FACE_OUTER_BOUND('',#1688,.T.);
#1218=FACE_OUTER_BOUND('',#1689,.T.);
#1219=FACE_OUTER_BOUND('',#1690,.T.);
#1220=FACE_OUTER_BOUND('',#1692,.T.);
#1221=FACE_OUTER_BOUND('',#1693,.T.);
#1222=FACE_OUTER_BOUND('',#1694,.T.);
#1223=FACE_OUTER_BOUND('',#1696,.T.);
#1224=EDGE_LOOP('',(#4504,#4505,#4506,#4507));
#1225=EDGE_LOOP('',(#4508,#4509,#4510,#4511));
#1226=EDGE_LOOP('',(#4512,#4513,#4514,#4515));
#1227=EDGE_LOOP('',(#4516,#4517,#4518));
#1228=EDGE_LOOP('',(#4519,#4520,#4521,#4522));
#1229=EDGE_LOOP('',(#4523,#4524,#4525));
#1230=EDGE_LOOP('',(#4526,#4527,#4528,#4529));
#1231=EDGE_LOOP('',(#4530,#4531,#4532,#4533));
#1232=EDGE_LOOP('',(#4534,#4535,#4536,#4537));
#1233=EDGE_LOOP('',(#4538,#4539,#4540,#4541));
#1234=EDGE_LOOP('',(#4542,#4543,#4544,#4545,#4546,#4547,#4548,#4549,#4550));
#1235=EDGE_LOOP('',(#4551,#4552,#4553,#4554,#4555,#4556));
#1236=EDGE_LOOP('',(#4557,#4558,#4559,#4560,#4561,#4562));
#1237=EDGE_LOOP('',(#4563,#4564,#4565,#4566));
#1238=EDGE_LOOP('',(#4567,#4568,#4569,#4570));
#1239=EDGE_LOOP('',(#4571,#4572,#4573,#4574));
#1240=EDGE_LOOP('',(#4575,#4576,#4577,#4578));
#1241=EDGE_LOOP('',(#4579,#4580,#4581,#4582,#4583,#4584,#4585,#4586,#4587,
#4588,#4589,#4590,#4591,#4592,#4593,#4594));
#1242=EDGE_LOOP('',(#4595));
#1243=EDGE_LOOP('',(#4596));
#1244=EDGE_LOOP('',(#4597));
#1245=EDGE_LOOP('',(#4598));
#1246=EDGE_LOOP('',(#4599,#4600,#4601,#4602));
#1247=EDGE_LOOP('',(#4603,#4604,#4605,#4606,#4607));
#1248=EDGE_LOOP('',(#4608,#4609,#4610,#4611,#4612,#4613,#4614,#4615,#4616,
#4617,#4618,#4619,#4620,#4621,#4622,#4623,#4624,#4625,#4626,#4627,#4628));
#1249=EDGE_LOOP('',(#4629));
#1250=EDGE_LOOP('',(#4630));
#1251=EDGE_LOOP('',(#4631));
#1252=EDGE_LOOP('',(#4632));
#1253=EDGE_LOOP('',(#4633,#4634,#4635,#4636,#4637));
#1254=EDGE_LOOP('',(#4638,#4639,#4640,#4641));
#1255=EDGE_LOOP('',(#4642,#4643,#4644,#4645));
#1256=EDGE_LOOP('',(#4646,#4647,#4648,#4649));
#1257=EDGE_LOOP('',(#4650,#4651,#4652,#4653));
#1258=EDGE_LOOP('',(#4654,#4655,#4656,#4657));
#1259=EDGE_LOOP('',(#4658,#4659,#4660,#4661));
#1260=EDGE_LOOP('',(#4662,#4663,#4664,#4665));
#1261=EDGE_LOOP('',(#4666,#4667,#4668,#4669));
#1262=EDGE_LOOP('',(#4670,#4671,#4672,#4673));
#1263=EDGE_LOOP('',(#4674,#4675,#4676,#4677));
#1264=EDGE_LOOP('',(#4678,#4679,#4680,#4681));
#1265=EDGE_LOOP('',(#4682,#4683,#4684,#4685));
#1266=EDGE_LOOP('',(#4686,#4687,#4688,#4689));
#1267=EDGE_LOOP('',(#4690,#4691,#4692,#4693));
#1268=EDGE_LOOP('',(#4694,#4695,#4696,#4697));
#1269=EDGE_LOOP('',(#4698,#4699,#4700,#4701));
#1270=EDGE_LOOP('',(#4702,#4703,#4704,#4705));
#1271=EDGE_LOOP('',(#4706,#4707,#4708,#4709));
#1272=EDGE_LOOP('',(#4710,#4711,#4712,#4713,#4714,#4715,#4716));
#1273=EDGE_LOOP('',(#4717,#4718,#4719,#4720,#4721,#4722));
#1274=EDGE_LOOP('',(#4723,#4724,#4725,#4726));
#1275=EDGE_LOOP('',(#4727,#4728,#4729,#4730,#4731));
#1276=EDGE_LOOP('',(#4732,#4733,#4734,#4735));
#1277=EDGE_LOOP('',(#4736,#4737,#4738,#4739));
#1278=EDGE_LOOP('',(#4740,#4741,#4742,#4743));
#1279=EDGE_LOOP('',(#4744,#4745,#4746,#4747,#4748,#4749,#4750,#4751,#4752,
#4753,#4754,#4755,#4756,#4757,#4758,#4759));
#1280=EDGE_LOOP('',(#4760));
#1281=EDGE_LOOP('',(#4761));
#1282=EDGE_LOOP('',(#4762));
#1283=EDGE_LOOP('',(#4763));
#1284=EDGE_LOOP('',(#4764,#4765,#4766,#4767));
#1285=EDGE_LOOP('',(#4768,#4769,#4770,#4771,#4772));
#1286=EDGE_LOOP('',(#4773,#4774,#4775,#4776,#4777,#4778,#4779,#4780,#4781,
#4782,#4783,#4784,#4785,#4786,#4787,#4788,#4789,#4790,#4791,#4792));
#1287=EDGE_LOOP('',(#4793));
#1288=EDGE_LOOP('',(#4794));
#1289=EDGE_LOOP('',(#4795));
#1290=EDGE_LOOP('',(#4796));
#1291=EDGE_LOOP('',(#4797,#4798,#4799,#4800,#4801));
#1292=EDGE_LOOP('',(#4802,#4803,#4804,#4805));
#1293=EDGE_LOOP('',(#4806,#4807,#4808,#4809));
#1294=EDGE_LOOP('',(#4810,#4811,#4812,#4813));
#1295=EDGE_LOOP('',(#4814,#4815,#4816,#4817));
#1296=EDGE_LOOP('',(#4818,#4819,#4820,#4821));
#1297=EDGE_LOOP('',(#4822,#4823,#4824,#4825));
#1298=EDGE_LOOP('',(#4826,#4827,#4828,#4829));
#1299=EDGE_LOOP('',(#4830,#4831,#4832,#4833));
#1300=EDGE_LOOP('',(#4834,#4835,#4836,#4837));
#1301=EDGE_LOOP('',(#4838,#4839,#4840,#4841));
#1302=EDGE_LOOP('',(#4842,#4843,#4844,#4845));
#1303=EDGE_LOOP('',(#4846));
#1304=EDGE_LOOP('',(#4847));
#1305=EDGE_LOOP('',(#4848));
#1306=EDGE_LOOP('',(#4849));
#1307=EDGE_LOOP('',(#4850,#4851,#4852,#4853));
#1308=EDGE_LOOP('',(#4854));
#1309=EDGE_LOOP('',(#4855));
#1310=EDGE_LOOP('',(#4856,#4857,#4858,#4859));
#1311=EDGE_LOOP('',(#4860));
#1312=EDGE_LOOP('',(#4861,#4862,#4863,#4864));
#1313=EDGE_LOOP('',(#4865));
#1314=EDGE_LOOP('',(#4866,#4867,#4868,#4869));
#1315=EDGE_LOOP('',(#4870,#4871,#4872,#4873));
#1316=EDGE_LOOP('',(#4874,#4875,#4876,#4877));
#1317=EDGE_LOOP('',(#4878,#4879,#4880,#4881));
#1318=EDGE_LOOP('',(#4882,#4883,#4884,#4885));
#1319=EDGE_LOOP('',(#4886,#4887,#4888,#4889));
#1320=EDGE_LOOP('',(#4890,#4891,#4892,#4893,#4894,#4895,#4896,#4897));
#1321=EDGE_LOOP('',(#4898));
#1322=EDGE_LOOP('',(#4899));
#1323=EDGE_LOOP('',(#4900));
#1324=EDGE_LOOP('',(#4901,#4902,#4903,#4904));
#1325=EDGE_LOOP('',(#4905,#4906,#4907,#4908));
#1326=EDGE_LOOP('',(#4909,#4910,#4911,#4912));
#1327=EDGE_LOOP('',(#4913,#4914,#4915,#4916));
#1328=EDGE_LOOP('',(#4917,#4918,#4919,#4920));
#1329=EDGE_LOOP('',(#4921));
#1330=EDGE_LOOP('',(#4922));
#1331=EDGE_LOOP('',(#4923,#4924,#4925,#4926));
#1332=EDGE_LOOP('',(#4927));
#1333=EDGE_LOOP('',(#4928));
#1334=EDGE_LOOP('',(#4929,#4930,#4931,#4932));
#1335=EDGE_LOOP('',(#4933,#4934,#4935,#4936));
#1336=EDGE_LOOP('',(#4937,#4938,#4939,#4940));
#1337=EDGE_LOOP('',(#4941,#4942,#4943,#4944));
#1338=EDGE_LOOP('',(#4945,#4946,#4947,#4948));
#1339=EDGE_LOOP('',(#4949,#4950,#4951,#4952));
#1340=EDGE_LOOP('',(#4953,#4954,#4955,#4956));
#1341=EDGE_LOOP('',(#4957,#4958,#4959,#4960));
#1342=EDGE_LOOP('',(#4961,#4962,#4963,#4964));
#1343=EDGE_LOOP('',(#4965));
#1344=EDGE_LOOP('',(#4966));
#1345=EDGE_LOOP('',(#4967));
#1346=EDGE_LOOP('',(#4968));
#1347=EDGE_LOOP('',(#4969,#4970,#4971,#4972));
#1348=EDGE_LOOP('',(#4973,#4974,#4975,#4976));
#1349=EDGE_LOOP('',(#4977,#4978,#4979,#4980));
#1350=EDGE_LOOP('',(#4981,#4982,#4983,#4984));
#1351=EDGE_LOOP('',(#4985,#4986,#4987,#4988));
#1352=EDGE_LOOP('',(#4989,#4990,#4991,#4992,#4993,#4994));
#1353=EDGE_LOOP('',(#4995,#4996,#4997,#4998,#4999,#5000,#5001,#5002,#5003,
#5004));
#1354=EDGE_LOOP('',(#5005,#5006,#5007,#5008,#5009,#5010,#5011,#5012,#5013,
#5014));
#1355=EDGE_LOOP('',(#5015,#5016,#5017,#5018,#5019,#5020,#5021,#5022,#5023,
#5024));
#1356=EDGE_LOOP('',(#5025,#5026,#5027,#5028,#5029,#5030,#5031,#5032));
#1357=EDGE_LOOP('',(#5033,#5034,#5035,#5036,#5037,#5038,#5039,#5040,#5041,
#5042,#5043,#5044,#5045,#5046,#5047,#5048,#5049,#5050,#5051,#5052,#5053,
#5054,#5055,#5056,#5057,#5058,#5059,#5060,#5061,#5062,#5063,#5064,#5065,
#5066,#5067,#5068,#5069,#5070,#5071,#5072,#5073,#5074));
#1358=EDGE_LOOP('',(#5075,#5076,#5077,#5078,#5079,#5080));
#1359=EDGE_LOOP('',(#5081,#5082,#5083,#5084));
#1360=EDGE_LOOP('',(#5085,#5086,#5087,#5088));
#1361=EDGE_LOOP('',(#5089,#5090,#5091,#5092,#5093,#5094));
#1362=EDGE_LOOP('',(#5095,#5096,#5097,#5098));
#1363=EDGE_LOOP('',(#5099,#5100,#5101,#5102));
#1364=EDGE_LOOP('',(#5103,#5104,#5105,#5106));
#1365=EDGE_LOOP('',(#5107,#5108,#5109,#5110));
#1366=EDGE_LOOP('',(#5111,#5112,#5113,#5114));
#1367=EDGE_LOOP('',(#5115));
#1368=EDGE_LOOP('',(#5116));
#1369=EDGE_LOOP('',(#5117));
#1370=EDGE_LOOP('',(#5118,#5119,#5120,#5121));
#1371=EDGE_LOOP('',(#5122,#5123,#5124,#5125));
#1372=EDGE_LOOP('',(#5126,#5127,#5128,#5129));
#1373=EDGE_LOOP('',(#5130,#5131,#5132,#5133));
#1374=EDGE_LOOP('',(#5134,#5135,#5136,#5137,#5138,#5139,#5140,#5141,#5142,
#5143));
#1375=EDGE_LOOP('',(#5144,#5145,#5146,#5147));
#1376=EDGE_LOOP('',(#5148,#5149,#5150,#5151));
#1377=EDGE_LOOP('',(#5152,#5153,#5154,#5155));
#1378=EDGE_LOOP('',(#5156,#5157,#5158,#5159));
#1379=EDGE_LOOP('',(#5160,#5161,#5162,#5163));
#1380=EDGE_LOOP('',(#5164,#5165,#5166,#5167,#5168,#5169,#5170,#5171,#5172,
#5173));
#1381=EDGE_LOOP('',(#5174,#5175,#5176,#5177));
#1382=EDGE_LOOP('',(#5178,#5179,#5180,#5181,#5182,#5183));
#1383=EDGE_LOOP('',(#5184,#5185,#5186,#5187,#5188,#5189));
#1384=EDGE_LOOP('',(#5190,#5191,#5192,#5193));
#1385=EDGE_LOOP('',(#5194,#5195,#5196,#5197,#5198,#5199,#5200,#5201,#5202,
#5203));
#1386=EDGE_LOOP('',(#5204,#5205,#5206,#5207));
#1387=EDGE_LOOP('',(#5208,#5209,#5210,#5211));
#1388=EDGE_LOOP('',(#5212,#5213,#5214,#5215));
#1389=EDGE_LOOP('',(#5216,#5217,#5218,#5219));
#1390=EDGE_LOOP('',(#5220,#5221,#5222,#5223));
#1391=EDGE_LOOP('',(#5224,#5225,#5226));
#1392=EDGE_LOOP('',(#5227,#5228,#5229));
#1393=EDGE_LOOP('',(#5230,#5231,#5232));
#1394=EDGE_LOOP('',(#5233,#5234,#5235,#5236));
#1395=EDGE_LOOP('',(#5237,#5238,#5239,#5240));
#1396=EDGE_LOOP('',(#5241,#5242,#5243));
#1397=EDGE_LOOP('',(#5244,#5245,#5246,#5247));
#1398=EDGE_LOOP('',(#5248,#5249,#5250,#5251));
#1399=EDGE_LOOP('',(#5252,#5253,#5254,#5255));
#1400=EDGE_LOOP('',(#5256,#5257,#5258,#5259));
#1401=EDGE_LOOP('',(#5260,#5261,#5262,#5263));
#1402=EDGE_LOOP('',(#5264,#5265,#5266,#5267));
#1403=EDGE_LOOP('',(#5268,#5269,#5270));
#1404=EDGE_LOOP('',(#5271,#5272,#5273));
#1405=EDGE_LOOP('',(#5274,#5275,#5276));
#1406=EDGE_LOOP('',(#5277,#5278,#5279,#5280));
#1407=EDGE_LOOP('',(#5281,#5282,#5283,#5284));
#1408=EDGE_LOOP('',(#5285,#5286,#5287));
#1409=EDGE_LOOP('',(#5288,#5289,#5290,#5291));
#1410=EDGE_LOOP('',(#5292,#5293,#5294,#5295));
#1411=EDGE_LOOP('',(#5296,#5297,#5298,#5299));
#1412=EDGE_LOOP('',(#5300,#5301,#5302,#5303));
#1413=EDGE_LOOP('',(#5304,#5305,#5306,#5307));
#1414=EDGE_LOOP('',(#5308,#5309,#5310,#5311));
#1415=EDGE_LOOP('',(#5312,#5313,#5314,#5315));
#1416=EDGE_LOOP('',(#5316,#5317,#5318,#5319,#5320,#5321,#5322,#5323));
#1417=EDGE_LOOP('',(#5324,#5325,#5326,#5327));
#1418=EDGE_LOOP('',(#5328));
#1419=EDGE_LOOP('',(#5329));
#1420=EDGE_LOOP('',(#5330));
#1421=EDGE_LOOP('',(#5331));
#1422=EDGE_LOOP('',(#5332));
#1423=EDGE_LOOP('',(#5333));
#1424=EDGE_LOOP('',(#5334,#5335,#5336,#5337));
#1425=EDGE_LOOP('',(#5338,#5339,#5340,#5341));
#1426=EDGE_LOOP('',(#5342,#5343,#5344,#5345,#5346,#5347,#5348,#5349));
#1427=EDGE_LOOP('',(#5350));
#1428=EDGE_LOOP('',(#5351));
#1429=EDGE_LOOP('',(#5352));
#1430=EDGE_LOOP('',(#5353,#5354,#5355,#5356));
#1431=EDGE_LOOP('',(#5357,#5358,#5359,#5360));
#1432=EDGE_LOOP('',(#5361,#5362,#5363,#5364));
#1433=EDGE_LOOP('',(#5365,#5366,#5367,#5368));
#1434=EDGE_LOOP('',(#5369,#5370,#5371,#5372));
#1435=EDGE_LOOP('',(#5373,#5374,#5375,#5376));
#1436=EDGE_LOOP('',(#5377,#5378,#5379,#5380));
#1437=EDGE_LOOP('',(#5381,#5382,#5383,#5384));
#1438=EDGE_LOOP('',(#5385,#5386,#5387,#5388));
#1439=EDGE_LOOP('',(#5389,#5390,#5391,#5392));
#1440=EDGE_LOOP('',(#5393,#5394,#5395,#5396,#5397,#5398));
#1441=EDGE_LOOP('',(#5399));
#1442=EDGE_LOOP('',(#5400,#5401,#5402,#5403));
#1443=EDGE_LOOP('',(#5404,#5405,#5406,#5407));
#1444=EDGE_LOOP('',(#5408,#5409,#5410,#5411));
#1445=EDGE_LOOP('',(#5412,#5413,#5414,#5415));
#1446=EDGE_LOOP('',(#5416,#5417,#5418,#5419));
#1447=EDGE_LOOP('',(#5420,#5421,#5422,#5423));
#1448=EDGE_LOOP('',(#5424,#5425,#5426,#5427,#5428,#5429));
#1449=EDGE_LOOP('',(#5430));
#1450=EDGE_LOOP('',(#5431,#5432,#5433,#5434));
#1451=EDGE_LOOP('',(#5435,#5436,#5437,#5438));
#1452=EDGE_LOOP('',(#5439,#5440,#5441,#5442));
#1453=EDGE_LOOP('',(#5443,#5444,#5445,#5446));
#1454=EDGE_LOOP('',(#5447,#5448,#5449,#5450));
#1455=EDGE_LOOP('',(#5451,#5452,#5453,#5454));
#1456=EDGE_LOOP('',(#5455,#5456,#5457,#5458));
#1457=EDGE_LOOP('',(#5459,#5460,#5461,#5462));
#1458=EDGE_LOOP('',(#5463,#5464,#5465,#5466));
#1459=EDGE_LOOP('',(#5467));
#1460=EDGE_LOOP('',(#5468));
#1461=EDGE_LOOP('',(#5469));
#1462=EDGE_LOOP('',(#5470));
#1463=EDGE_LOOP('',(#5471,#5472,#5473,#5474));
#1464=EDGE_LOOP('',(#5475,#5476,#5477,#5478));
#1465=EDGE_LOOP('',(#5479,#5480,#5481,#5482));
#1466=EDGE_LOOP('',(#5483,#5484,#5485,#5486));
#1467=EDGE_LOOP('',(#5487,#5488,#5489,#5490));
#1468=EDGE_LOOP('',(#5491,#5492,#5493,#5494,#5495,#5496));
#1469=EDGE_LOOP('',(#5497,#5498,#5499,#5500,#5501,#5502,#5503,#5504,#5505,
#5506));
#1470=EDGE_LOOP('',(#5507,#5508,#5509,#5510,#5511,#5512,#5513,#5514,#5515,
#5516));
#1471=EDGE_LOOP('',(#5517,#5518,#5519,#5520,#5521,#5522,#5523,#5524,#5525,
#5526));
#1472=EDGE_LOOP('',(#5527,#5528,#5529,#5530,#5531,#5532,#5533,#5534));
#1473=EDGE_LOOP('',(#5535,#5536,#5537,#5538,#5539,#5540,#5541,#5542,#5543,
#5544,#5545,#5546,#5547,#5548,#5549,#5550,#5551,#5552,#5553,#5554,#5555,
#5556,#5557,#5558,#5559,#5560,#5561,#5562,#5563,#5564,#5565,#5566,#5567,
#5568,#5569,#5570,#5571,#5572,#5573,#5574,#5575,#5576));
#1474=EDGE_LOOP('',(#5577,#5578,#5579,#5580,#5581,#5582));
#1475=EDGE_LOOP('',(#5583,#5584,#5585,#5586));
#1476=EDGE_LOOP('',(#5587,#5588,#5589,#5590));
#1477=EDGE_LOOP('',(#5591,#5592,#5593,#5594,#5595,#5596));
#1478=EDGE_LOOP('',(#5597,#5598,#5599,#5600));
#1479=EDGE_LOOP('',(#5601,#5602,#5603,#5604));
#1480=EDGE_LOOP('',(#5605,#5606,#5607,#5608));
#1481=EDGE_LOOP('',(#5609,#5610,#5611,#5612));
#1482=EDGE_LOOP('',(#5613,#5614,#5615,#5616));
#1483=EDGE_LOOP('',(#5617));
#1484=EDGE_LOOP('',(#5618));
#1485=EDGE_LOOP('',(#5619));
#1486=EDGE_LOOP('',(#5620,#5621,#5622,#5623));
#1487=EDGE_LOOP('',(#5624,#5625,#5626,#5627));
#1488=EDGE_LOOP('',(#5628,#5629,#5630,#5631));
#1489=EDGE_LOOP('',(#5632,#5633,#5634,#5635));
#1490=EDGE_LOOP('',(#5636,#5637,#5638,#5639,#5640,#5641,#5642,#5643,#5644,
#5645));
#1491=EDGE_LOOP('',(#5646,#5647,#5648,#5649));
#1492=EDGE_LOOP('',(#5650,#5651,#5652,#5653));
#1493=EDGE_LOOP('',(#5654,#5655,#5656,#5657));
#1494=EDGE_LOOP('',(#5658,#5659,#5660,#5661));
#1495=EDGE_LOOP('',(#5662,#5663,#5664,#5665));
#1496=EDGE_LOOP('',(#5666,#5667,#5668,#5669,#5670,#5671,#5672,#5673,#5674,
#5675));
#1497=EDGE_LOOP('',(#5676,#5677,#5678,#5679));
#1498=EDGE_LOOP('',(#5680,#5681,#5682,#5683,#5684,#5685));
#1499=EDGE_LOOP('',(#5686,#5687,#5688,#5689,#5690,#5691));
#1500=EDGE_LOOP('',(#5692,#5693,#5694,#5695));
#1501=EDGE_LOOP('',(#5696,#5697,#5698,#5699,#5700,#5701,#5702,#5703,#5704,
#5705));
#1502=EDGE_LOOP('',(#5706,#5707,#5708,#5709));
#1503=EDGE_LOOP('',(#5710,#5711,#5712,#5713));
#1504=EDGE_LOOP('',(#5714,#5715,#5716,#5717));
#1505=EDGE_LOOP('',(#5718,#5719,#5720,#5721));
#1506=EDGE_LOOP('',(#5722,#5723,#5724,#5725));
#1507=EDGE_LOOP('',(#5726,#5727,#5728));
#1508=EDGE_LOOP('',(#5729,#5730,#5731));
#1509=EDGE_LOOP('',(#5732,#5733,#5734));
#1510=EDGE_LOOP('',(#5735,#5736,#5737,#5738));
#1511=EDGE_LOOP('',(#5739,#5740,#5741,#5742));
#1512=EDGE_LOOP('',(#5743,#5744,#5745));
#1513=EDGE_LOOP('',(#5746,#5747,#5748,#5749));
#1514=EDGE_LOOP('',(#5750,#5751,#5752,#5753));
#1515=EDGE_LOOP('',(#5754,#5755,#5756,#5757));
#1516=EDGE_LOOP('',(#5758,#5759,#5760,#5761));
#1517=EDGE_LOOP('',(#5762,#5763,#5764,#5765));
#1518=EDGE_LOOP('',(#5766,#5767,#5768,#5769));
#1519=EDGE_LOOP('',(#5770,#5771,#5772));
#1520=EDGE_LOOP('',(#5773,#5774,#5775));
#1521=EDGE_LOOP('',(#5776,#5777,#5778));
#1522=EDGE_LOOP('',(#5779,#5780,#5781,#5782));
#1523=EDGE_LOOP('',(#5783,#5784,#5785,#5786));
#1524=EDGE_LOOP('',(#5787,#5788,#5789));
#1525=EDGE_LOOP('',(#5790,#5791,#5792,#5793));
#1526=EDGE_LOOP('',(#5794,#5795,#5796,#5797));
#1527=EDGE_LOOP('',(#5798,#5799,#5800,#5801));
#1528=EDGE_LOOP('',(#5802,#5803,#5804,#5805));
#1529=EDGE_LOOP('',(#5806,#5807,#5808,#5809));
#1530=EDGE_LOOP('',(#5810,#5811,#5812,#5813));
#1531=EDGE_LOOP('',(#5814,#5815,#5816,#5817));
#1532=EDGE_LOOP('',(#5818,#5819,#5820,#5821,#5822,#5823,#5824,#5825));
#1533=EDGE_LOOP('',(#5826,#5827,#5828,#5829));
#1534=EDGE_LOOP('',(#5830,#5831,#5832,#5833,#5834,#5835));
#1535=EDGE_LOOP('',(#5836,#5837,#5838,#5839,#5840,#5841));
#1536=EDGE_LOOP('',(#5842));
#1537=EDGE_LOOP('',(#5843));
#1538=EDGE_LOOP('',(#5844));
#1539=EDGE_LOOP('',(#5845));
#1540=EDGE_LOOP('',(#5846,#5847,#5848,#5849));
#1541=EDGE_LOOP('',(#5850,#5851,#5852,#5853));
#1542=EDGE_LOOP('',(#5854,#5855,#5856,#5857));
#1543=EDGE_LOOP('',(#5858,#5859,#5860,#5861));
#1544=EDGE_LOOP('',(#5862));
#1545=EDGE_LOOP('',(#5863));
#1546=EDGE_LOOP('',(#5864,#5865,#5866,#5867));
#1547=EDGE_LOOP('',(#5868));
#1548=EDGE_LOOP('',(#5869));
#1549=EDGE_LOOP('',(#5870));
#1550=EDGE_LOOP('',(#5871,#5872,#5873,#5874));
#1551=EDGE_LOOP('',(#5875));
#1552=EDGE_LOOP('',(#5876));
#1553=EDGE_LOOP('',(#5877));
#1554=EDGE_LOOP('',(#5878,#5879,#5880,#5881));
#1555=EDGE_LOOP('',(#5882));
#1556=EDGE_LOOP('',(#5883));
#1557=EDGE_LOOP('',(#5884));
#1558=EDGE_LOOP('',(#5885,#5886,#5887,#5888));
#1559=EDGE_LOOP('',(#5889));
#1560=EDGE_LOOP('',(#5890,#5891,#5892,#5893));
#1561=EDGE_LOOP('',(#5894,#5895,#5896,#5897));
#1562=EDGE_LOOP('',(#5898,#5899,#5900,#5901));
#1563=EDGE_LOOP('',(#5902,#5903,#5904,#5905));
#1564=EDGE_LOOP('',(#5906,#5907,#5908,#5909));
#1565=EDGE_LOOP('',(#5910,#5911,#5912,#5913));
#1566=EDGE_LOOP('',(#5914,#5915,#5916,#5917));
#1567=EDGE_LOOP('',(#5918,#5919,#5920,#5921));
#1568=EDGE_LOOP('',(#5922,#5923,#5924,#5925));
#1569=EDGE_LOOP('',(#5926,#5927,#5928,#5929));
#1570=EDGE_LOOP('',(#5930,#5931,#5932,#5933));
#1571=EDGE_LOOP('',(#5934,#5935,#5936,#5937));
#1572=EDGE_LOOP('',(#5938,#5939,#5940,#5941));
#1573=EDGE_LOOP('',(#5942,#5943,#5944,#5945));
#1574=EDGE_LOOP('',(#5946,#5947,#5948,#5949));
#1575=EDGE_LOOP('',(#5950,#5951,#5952,#5953));
#1576=EDGE_LOOP('',(#5954,#5955,#5956,#5957,#5958,#5959,#5960,#5961));
#1577=EDGE_LOOP('',(#5962));
#1578=EDGE_LOOP('',(#5963));
#1579=EDGE_LOOP('',(#5964,#5965,#5966,#5967));
#1580=EDGE_LOOP('',(#5968,#5969,#5970,#5971));
#1581=EDGE_LOOP('',(#5972,#5973,#5974,#5975));
#1582=EDGE_LOOP('',(#5976,#5977,#5978,#5979,#5980,#5981,#5982,#5983));
#1583=EDGE_LOOP('',(#5984));
#1584=EDGE_LOOP('',(#5985));
#1585=EDGE_LOOP('',(#5986));
#1586=EDGE_LOOP('',(#5987));
#1587=EDGE_LOOP('',(#5988));
#1588=EDGE_LOOP('',(#5989));
#1589=EDGE_LOOP('',(#5990,#5991,#5992,#5993));
#1590=EDGE_LOOP('',(#5994,#5995,#5996,#5997));
#1591=EDGE_LOOP('',(#5998,#5999,#6000,#6001));
#1592=EDGE_LOOP('',(#6002,#6003,#6004,#6005));
#1593=EDGE_LOOP('',(#6006,#6007,#6008,#6009));
#1594=EDGE_LOOP('',(#6010,#6011,#6012,#6013));
#1595=EDGE_LOOP('',(#6014,#6015,#6016,#6017));
#1596=EDGE_LOOP('',(#6018,#6019,#6020,#6021));
#1597=EDGE_LOOP('',(#6022,#6023,#6024,#6025));
#1598=EDGE_LOOP('',(#6026,#6027,#6028,#6029));
#1599=EDGE_LOOP('',(#6030,#6031,#6032,#6033));
#1600=EDGE_LOOP('',(#6034,#6035,#6036,#6037));
#1601=EDGE_LOOP('',(#6038,#6039,#6040,#6041));
#1602=EDGE_LOOP('',(#6042,#6043,#6044,#6045));
#1603=EDGE_LOOP('',(#6046,#6047,#6048,#6049));
#1604=EDGE_LOOP('',(#6050,#6051,#6052,#6053));
#1605=EDGE_LOOP('',(#6054,#6055,#6056,#6057));
#1606=EDGE_LOOP('',(#6058,#6059,#6060,#6061));
#1607=EDGE_LOOP('',(#6062,#6063,#6064,#6065));
#1608=EDGE_LOOP('',(#6066,#6067,#6068,#6069));
#1609=EDGE_LOOP('',(#6070,#6071,#6072,#6073));
#1610=EDGE_LOOP('',(#6074,#6075,#6076,#6077));
#1611=EDGE_LOOP('',(#6078,#6079,#6080,#6081));
#1612=EDGE_LOOP('',(#6082,#6083,#6084,#6085));
#1613=EDGE_LOOP('',(#6086,#6087,#6088,#6089));
#1614=EDGE_LOOP('',(#6090,#6091,#6092,#6093));
#1615=EDGE_LOOP('',(#6094,#6095,#6096,#6097));
#1616=EDGE_LOOP('',(#6098,#6099,#6100,#6101));
#1617=EDGE_LOOP('',(#6102,#6103,#6104,#6105));
#1618=EDGE_LOOP('',(#6106,#6107,#6108,#6109));
#1619=EDGE_LOOP('',(#6110,#6111,#6112,#6113));
#1620=EDGE_LOOP('',(#6114,#6115,#6116,#6117));
#1621=EDGE_LOOP('',(#6118,#6119,#6120,#6121));
#1622=EDGE_LOOP('',(#6122,#6123,#6124,#6125));
#1623=EDGE_LOOP('',(#6126,#6127,#6128,#6129));
#1624=EDGE_LOOP('',(#6130,#6131,#6132,#6133));
#1625=EDGE_LOOP('',(#6134,#6135,#6136,#6137));
#1626=EDGE_LOOP('',(#6138,#6139,#6140,#6141));
#1627=EDGE_LOOP('',(#6142,#6143,#6144,#6145));
#1628=EDGE_LOOP('',(#6146,#6147,#6148,#6149));
#1629=EDGE_LOOP('',(#6150,#6151,#6152,#6153));
#1630=EDGE_LOOP('',(#6154,#6155,#6156,#6157));
#1631=EDGE_LOOP('',(#6158,#6159,#6160,#6161));
#1632=EDGE_LOOP('',(#6162,#6163,#6164,#6165));
#1633=EDGE_LOOP('',(#6166,#6167,#6168,#6169));
#1634=EDGE_LOOP('',(#6170,#6171,#6172,#6173));
#1635=EDGE_LOOP('',(#6174,#6175,#6176,#6177));
#1636=EDGE_LOOP('',(#6178,#6179,#6180,#6181));
#1637=EDGE_LOOP('',(#6182,#6183,#6184,#6185));
#1638=EDGE_LOOP('',(#6186,#6187,#6188,#6189));
#1639=EDGE_LOOP('',(#6190,#6191,#6192,#6193));
#1640=EDGE_LOOP('',(#6194,#6195,#6196,#6197));
#1641=EDGE_LOOP('',(#6198,#6199,#6200,#6201));
#1642=EDGE_LOOP('',(#6202,#6203,#6204,#6205));
#1643=EDGE_LOOP('',(#6206,#6207,#6208,#6209));
#1644=EDGE_LOOP('',(#6210,#6211,#6212,#6213));
#1645=EDGE_LOOP('',(#6214,#6215,#6216,#6217));
#1646=EDGE_LOOP('',(#6218,#6219,#6220,#6221));
#1647=EDGE_LOOP('',(#6222,#6223,#6224,#6225));
#1648=EDGE_LOOP('',(#6226,#6227,#6228,#6229));
#1649=EDGE_LOOP('',(#6230,#6231,#6232,#6233));
#1650=EDGE_LOOP('',(#6234,#6235,#6236,#6237,#6238,#6239,#6240,#6241));
#1651=EDGE_LOOP('',(#6242,#6243,#6244,#6245,#6246,#6247,#6248,#6249,#6250,
#6251,#6252,#6253,#6254,#6255,#6256,#6257,#6258,#6259,#6260,#6261,#6262,
#6263,#6264,#6265,#6266,#6267,#6268,#6269,#6270,#6271,#6272,#6273,#6274,
#6275,#6276,#6277,#6278,#6279,#6280,#6281,#6282,#6283,#6284,#6285,#6286,
#6287,#6288,#6289,#6290,#6291,#6292,#6293,#6294,#6295,#6296,#6297,#6298,
#6299,#6300,#6301,#6302,#6303,#6304,#6305));
#1652=EDGE_LOOP('',(#6306,#6307,#6308,#6309));
#1653=EDGE_LOOP('',(#6310,#6311,#6312,#6313,#6314,#6315,#6316,#6317,#6318,
#6319,#6320,#6321,#6322,#6323,#6324,#6325,#6326,#6327,#6328,#6329,#6330,
#6331,#6332,#6333,#6334,#6335,#6336,#6337,#6338,#6339,#6340,#6341,#6342,
#6343,#6344,#6345,#6346,#6347,#6348,#6349,#6350,#6351,#6352,#6353,#6354,
#6355,#6356,#6357,#6358,#6359,#6360,#6361,#6362,#6363,#6364,#6365,#6366,
#6367,#6368,#6369,#6370,#6371,#6372,#6373,#6374));
#1654=EDGE_LOOP('',(#6375,#6376,#6377,#6378));
#1655=EDGE_LOOP('',(#6379,#6380,#6381,#6382));
#1656=EDGE_LOOP('',(#6383,#6384,#6385,#6386));
#1657=EDGE_LOOP('',(#6387,#6388,#6389,#6390));
#1658=EDGE_LOOP('',(#6391,#6392,#6393,#6394));
#1659=EDGE_LOOP('',(#6395,#6396,#6397,#6398));
#1660=EDGE_LOOP('',(#6399,#6400,#6401,#6402));
#1661=EDGE_LOOP('',(#6403,#6404,#6405,#6406,#6407,#6408));
#1662=EDGE_LOOP('',(#6409));
#1663=EDGE_LOOP('',(#6410,#6411,#6412,#6413));
#1664=EDGE_LOOP('',(#6414,#6415,#6416,#6417));
#1665=EDGE_LOOP('',(#6418));
#1666=EDGE_LOOP('',(#6419,#6420,#6421,#6422,#6423,#6424));
#1667=EDGE_LOOP('',(#6425));
#1668=EDGE_LOOP('',(#6426,#6427,#6428));
#1669=EDGE_LOOP('',(#6429,#6430,#6431,#6432,#6433));
#1670=EDGE_LOOP('',(#6434,#6435,#6436,#6437));
#1671=EDGE_LOOP('',(#6438,#6439,#6440,#6441));
#1672=EDGE_LOOP('',(#6442,#6443,#6444,#6445));
#1673=EDGE_LOOP('',(#6446,#6447,#6448,#6449));
#1674=EDGE_LOOP('',(#6450,#6451,#6452,#6453));
#1675=EDGE_LOOP('',(#6454,#6455,#6456,#6457));
#1676=EDGE_LOOP('',(#6458,#6459,#6460,#6461));
#1677=EDGE_LOOP('',(#6462,#6463,#6464,#6465));
#1678=EDGE_LOOP('',(#6466,#6467,#6468,#6469));
#1679=EDGE_LOOP('',(#6470,#6471,#6472,#6473,#6474,#6475,#6476,#6477,#6478,
#6479,#6480,#6481,#6482,#6483));
#1680=EDGE_LOOP('',(#6484,#6485,#6486,#6487,#6488,#6489,#6490,#6491,#6492,
#6493,#6494,#6495,#6496));
#1681=EDGE_LOOP('',(#6497,#6498,#6499,#6500,#6501,#6502));
#1682=EDGE_LOOP('',(#6503,#6504,#6505,#6506));
#1683=EDGE_LOOP('',(#6507,#6508,#6509,#6510));
#1684=EDGE_LOOP('',(#6511,#6512,#6513,#6514));
#1685=EDGE_LOOP('',(#6515,#6516,#6517,#6518));
#1686=EDGE_LOOP('',(#6519,#6520,#6521,#6522));
#1687=EDGE_LOOP('',(#6523,#6524,#6525,#6526));
#1688=EDGE_LOOP('',(#6527,#6528,#6529,#6530));
#1689=EDGE_LOOP('',(#6531,#6532,#6533,#6534));
#1690=EDGE_LOOP('',(#6535,#6536,#6537,#6538,#6539,#6540));
#1691=EDGE_LOOP('',(#6541,#6542,#6543,#6544,#6545));
#1692=EDGE_LOOP('',(#6546,#6547,#6548,#6549));
#1693=EDGE_LOOP('',(#6550,#6551,#6552,#6553));
#1694=EDGE_LOOP('',(#6554));
#1695=EDGE_LOOP('',(#6555));
#1696=EDGE_LOOP('',(#6556));
#1697=EDGE_LOOP('',(#6557));
#1698=LINE('',#9324,#2157);
#1699=LINE('',#9330,#2158);
#1700=LINE('',#9336,#2159);
#1701=LINE('',#9341,#2160);
#1702=LINE('',#9343,#2161);
#1703=LINE('',#9344,#2162);
#1704=LINE('',#9348,#2163);
#1705=LINE('',#9353,#2164);
#1706=LINE('',#9354,#2165);
#1707=LINE('',#9358,#2166);
#1708=LINE('',#9359,#2167);
#1709=LINE('',#9360,#2168);
#1710=LINE('',#9364,#2169);
#1711=LINE('',#9366,#2170);
#1712=LINE('',#9368,#2171);
#1713=LINE('',#9369,#2172);
#1714=LINE('',#9375,#2173);
#1715=LINE('',#9381,#2174);
#1716=LINE('',#9382,#2175);
#1717=LINE('',#9385,#2176);
#1718=LINE('',#9387,#2177);
#1719=LINE('',#9389,#2178);
#1720=LINE('',#9390,#2179);
#1721=LINE('',#9393,#2180);
#1722=LINE('',#9395,#2181);
#1723=LINE('',#9396,#2182);
#1724=LINE('',#9400,#2183);
#1725=LINE('',#9401,#2184);
#1726=LINE('',#9402,#2185);
#1727=LINE('',#9406,#2186);
#1728=LINE('',#9407,#2187);
#1729=LINE('',#9408,#2188);
#1730=LINE('',#9413,#2189);
#1731=LINE('',#9419,#2190);
#1732=LINE('',#9423,#2191);
#1733=LINE('',#9427,#2192);
#1734=LINE('',#9429,#2193);
#1735=LINE('',#9431,#2194);
#1736=LINE('',#9433,#2195);
#1737=LINE('',#9435,#2196);
#1738=LINE('',#9439,#2197);
#1739=LINE('',#9440,#2198);
#1740=LINE('',#9454,#2199);
#1741=LINE('',#9457,#2200);
#1742=LINE('',#9459,#2201);
#1743=LINE('',#9463,#2202);
#1744=LINE('',#9465,#2203);
#1745=LINE('',#9467,#2204);
#1746=LINE('',#9469,#2205);
#1747=LINE('',#9471,#2206);
#1748=LINE('',#9474,#2207);
#1749=LINE('',#9478,#2208);
#1750=LINE('',#9479,#2209);
#1751=LINE('',#9481,#2210);
#1752=LINE('',#9482,#2211);
#1753=LINE('',#9484,#2212);
#1754=LINE('',#9486,#2213);
#1755=LINE('',#9489,#2214);
#1756=LINE('',#9492,#2215);
#1757=LINE('',#9494,#2216);
#1758=LINE('',#9501,#2217);
#1759=LINE('',#9507,#2218);
#1760=LINE('',#9513,#2219);
#1761=LINE('',#9518,#2220);
#1762=LINE('',#9520,#2221);
#1763=LINE('',#9522,#2222);
#1764=LINE('',#9523,#2223);
#1765=LINE('',#9527,#2224);
#1766=LINE('',#9529,#2225);
#1767=LINE('',#9531,#2226);
#1768=LINE('',#9532,#2227);
#1769=LINE('',#9538,#2228);
#1770=LINE('',#9544,#2229);
#1771=LINE('',#9550,#2230);
#1772=LINE('',#9551,#2231);
#1773=LINE('',#9554,#2232);
#1774=LINE('',#9556,#2233);
#1775=LINE('',#9558,#2234);
#1776=LINE('',#9559,#2235);
#1777=LINE('',#9562,#2236);
#1778=LINE('',#9563,#2237);
#1779=LINE('',#9567,#2238);
#1780=LINE('',#9568,#2239);
#1781=LINE('',#9569,#2240);
#1782=LINE('',#9573,#2241);
#1783=LINE('',#9574,#2242);
#1784=LINE('',#9575,#2243);
#1785=LINE('',#9580,#2244);
#1786=LINE('',#9586,#2245);
#1787=LINE('',#9590,#2246);
#1788=LINE('',#9594,#2247);
#1789=LINE('',#9596,#2248);
#1790=LINE('',#9598,#2249);
#1791=LINE('',#9600,#2250);
#1792=LINE('',#9602,#2251);
#1793=LINE('',#9606,#2252);
#1794=LINE('',#9607,#2253);
#1795=LINE('',#9621,#2254);
#1796=LINE('',#9624,#2255);
#1797=LINE('',#9626,#2256);
#1798=LINE('',#9630,#2257);
#1799=LINE('',#9632,#2258);
#1800=LINE('',#9634,#2259);
#1801=LINE('',#9636,#2260);
#1802=LINE('',#9638,#2261);
#1803=LINE('',#9641,#2262);
#1804=LINE('',#9645,#2263);
#1805=LINE('',#9646,#2264);
#1806=LINE('',#9648,#2265);
#1807=LINE('',#9649,#2266);
#1808=LINE('',#9651,#2267);
#1809=LINE('',#9653,#2268);
#1810=LINE('',#9656,#2269);
#1811=LINE('',#9659,#2270);
#1812=LINE('',#9661,#2271);
#1813=LINE('',#9668,#2272);
#1814=LINE('',#9679,#2273);
#1815=LINE('',#9687,#2274);
#1816=LINE('',#9691,#2275);
#1817=LINE('',#9697,#2276);
#1818=LINE('',#9699,#2277);
#1819=LINE('',#9701,#2278);
#1820=LINE('',#9702,#2279);
#1821=LINE('',#9706,#2280);
#1822=LINE('',#9708,#2281);
#1823=LINE('',#9710,#2282);
#1824=LINE('',#9711,#2283);
#1825=LINE('',#9730,#2284);
#1826=LINE('',#9762,#2285);
#1827=LINE('',#9797,#2286);
#1828=LINE('',#9802,#2287);
#1829=LINE('',#9806,#2288);
#1830=LINE('',#9811,#2289);
#1831=LINE('',#9817,#2290);
#1832=LINE('',#9826,#2291);
#1833=LINE('',#9833,#2292);
#1834=LINE('',#9837,#2293);
#1835=LINE('',#9842,#2294);
#1836=LINE('',#9844,#2295);
#1837=LINE('',#9846,#2296);
#1838=LINE('',#9847,#2297);
#1839=LINE('',#9851,#2298);
#1840=LINE('',#9853,#2299);
#1841=LINE('',#9855,#2300);
#1842=LINE('',#9856,#2301);
#1843=LINE('',#9860,#2302);
#1844=LINE('',#9862,#2303);
#1845=LINE('',#9864,#2304);
#1846=LINE('',#9865,#2305);
#1847=LINE('',#9869,#2306);
#1848=LINE('',#9871,#2307);
#1849=LINE('',#9873,#2308);
#1850=LINE('',#9874,#2309);
#1851=LINE('',#9878,#2310);
#1852=LINE('',#9880,#2311);
#1853=LINE('',#9882,#2312);
#1854=LINE('',#9883,#2313);
#1855=LINE('',#9887,#2314);
#1856=LINE('',#9889,#2315);
#1857=LINE('',#9891,#2316);
#1858=LINE('',#9892,#2317);
#1859=LINE('',#9896,#2318);
#1860=LINE('',#9898,#2319);
#1861=LINE('',#9900,#2320);
#1862=LINE('',#9901,#2321);
#1863=LINE('',#9909,#2322);
#1864=LINE('',#9910,#2323);
#1865=LINE('',#9912,#2324);
#1866=LINE('',#9913,#2325);
#1867=LINE('',#9915,#2326);
#1868=LINE('',#9916,#2327);
#1869=LINE('',#9919,#2328);
#1870=LINE('',#9921,#2329);
#1871=LINE('',#9922,#2330);
#1872=LINE('',#9925,#2331);
#1873=LINE('',#9927,#2332);
#1874=LINE('',#9928,#2333);
#1875=LINE('',#9932,#2334);
#1876=LINE('',#9970,#2335);
#1877=LINE('',#10008,#2336);
#1878=LINE('',#10046,#2337);
#1879=LINE('',#10083,#2338);
#1880=LINE('',#10086,#2339);
#1881=LINE('',#10124,#2340);
#1882=LINE('',#10161,#2341);
#1883=LINE('',#10164,#2342);
#1884=LINE('',#10236,#2343);
#1885=LINE('',#10239,#2344);
#1886=LINE('',#10246,#2345);
#1887=LINE('',#10252,#2346);
#1888=LINE('',#10263,#2347);
#1889=LINE('',#10275,#2348);
#1890=LINE('',#10281,#2349);
#1891=LINE('',#10316,#2350);
#1892=LINE('',#10405,#2351);
#1893=LINE('',#10493,#2352);
#1894=LINE('',#10528,#2353);
#1895=LINE('',#10534,#2354);
#1896=LINE('',#10546,#2355);
#1897=LINE('',#10589,#2356);
#1898=LINE('',#10630,#2357);
#1899=LINE('',#10634,#2358);
#1900=LINE('',#10636,#2359);
#1901=LINE('',#10682,#2360);
#1902=LINE('',#10817,#2361);
#1903=LINE('',#10921,#2362);
#1904=LINE('',#11235,#2363);
#1905=LINE('',#11324,#2364);
#1906=LINE('',#11412,#2365);
#1907=LINE('',#11532,#2366);
#1908=LINE('',#11533,#2367);
#1909=LINE('',#11570,#2368);
#1910=LINE('',#11571,#2369);
#1911=LINE('',#11778,#2370);
#1912=LINE('',#11810,#2371);
#1913=LINE('',#11845,#2372);
#1914=LINE('',#11850,#2373);
#1915=LINE('',#11854,#2374);
#1916=LINE('',#11859,#2375);
#1917=LINE('',#11864,#2376);
#1918=LINE('',#11866,#2377);
#1919=LINE('',#11868,#2378);
#1920=LINE('',#11869,#2379);
#1921=LINE('',#11872,#2380);
#1922=LINE('',#11874,#2381);
#1923=LINE('',#11875,#2382);
#1924=LINE('',#11878,#2383);
#1925=LINE('',#11880,#2384);
#1926=LINE('',#11881,#2385);
#1927=LINE('',#11884,#2386);
#1928=LINE('',#11886,#2387);
#1929=LINE('',#11887,#2388);
#1930=LINE('',#11890,#2389);
#1931=LINE('',#11892,#2390);
#1932=LINE('',#11893,#2391);
#1933=LINE('',#11895,#2392);
#1934=LINE('',#11896,#2393);
#1935=LINE('',#11903,#2394);
#1936=LINE('',#11905,#2395);
#1937=LINE('',#11907,#2396);
#1938=LINE('',#11908,#2397);
#1939=LINE('',#11911,#2398);
#1940=LINE('',#11913,#2399);
#1941=LINE('',#11914,#2400);
#1942=LINE('',#11917,#2401);
#1943=LINE('',#11919,#2402);
#1944=LINE('',#11920,#2403);
#1945=LINE('',#11923,#2404);
#1946=LINE('',#11925,#2405);
#1947=LINE('',#11926,#2406);
#1948=LINE('',#11929,#2407);
#1949=LINE('',#11931,#2408);
#1950=LINE('',#11932,#2409);
#1951=LINE('',#11934,#2410);
#1952=LINE('',#11935,#2411);
#1953=LINE('',#11941,#2412);
#1954=LINE('',#11945,#2413);
#1955=LINE('',#11950,#2414);
#1956=LINE('',#11952,#2415);
#1957=LINE('',#11954,#2416);
#1958=LINE('',#11955,#2417);
#1959=LINE('',#11959,#2418);
#1960=LINE('',#11961,#2419);
#1961=LINE('',#11963,#2420);
#1962=LINE('',#11964,#2421);
#1963=LINE('',#11968,#2422);
#1964=LINE('',#11970,#2423);
#1965=LINE('',#11972,#2424);
#1966=LINE('',#11973,#2425);
#1967=LINE('',#11977,#2426);
#1968=LINE('',#11979,#2427);
#1969=LINE('',#11981,#2428);
#1970=LINE('',#11982,#2429);
#1971=LINE('',#11986,#2430);
#1972=LINE('',#11988,#2431);
#1973=LINE('',#11990,#2432);
#1974=LINE('',#11991,#2433);
#1975=LINE('',#11995,#2434);
#1976=LINE('',#11997,#2435);
#1977=LINE('',#11999,#2436);
#1978=LINE('',#12000,#2437);
#1979=LINE('',#12004,#2438);
#1980=LINE('',#12006,#2439);
#1981=LINE('',#12008,#2440);
#1982=LINE('',#12009,#2441);
#1983=LINE('',#12017,#2442);
#1984=LINE('',#12018,#2443);
#1985=LINE('',#12020,#2444);
#1986=LINE('',#12021,#2445);
#1987=LINE('',#12023,#2446);
#1988=LINE('',#12024,#2447);
#1989=LINE('',#12027,#2448);
#1990=LINE('',#12029,#2449);
#1991=LINE('',#12030,#2450);
#1992=LINE('',#12033,#2451);
#1993=LINE('',#12035,#2452);
#1994=LINE('',#12036,#2453);
#1995=LINE('',#12040,#2454);
#1996=LINE('',#12078,#2455);
#1997=LINE('',#12116,#2456);
#1998=LINE('',#12154,#2457);
#1999=LINE('',#12191,#2458);
#2000=LINE('',#12194,#2459);
#2001=LINE('',#12232,#2460);
#2002=LINE('',#12269,#2461);
#2003=LINE('',#12272,#2462);
#2004=LINE('',#12344,#2463);
#2005=LINE('',#12347,#2464);
#2006=LINE('',#12354,#2465);
#2007=LINE('',#12360,#2466);
#2008=LINE('',#12371,#2467);
#2009=LINE('',#12383,#2468);
#2010=LINE('',#12389,#2469);
#2011=LINE('',#12424,#2470);
#2012=LINE('',#12513,#2471);
#2013=LINE('',#12601,#2472);
#2014=LINE('',#12636,#2473);
#2015=LINE('',#12642,#2474);
#2016=LINE('',#12654,#2475);
#2017=LINE('',#12697,#2476);
#2018=LINE('',#12738,#2477);
#2019=LINE('',#12742,#2478);
#2020=LINE('',#12744,#2479);
#2021=LINE('',#12790,#2480);
#2022=LINE('',#12925,#2481);
#2023=LINE('',#13029,#2482);
#2024=LINE('',#13343,#2483);
#2025=LINE('',#13432,#2484);
#2026=LINE('',#13520,#2485);
#2027=LINE('',#13640,#2486);
#2028=LINE('',#13641,#2487);
#2029=LINE('',#13678,#2488);
#2030=LINE('',#13679,#2489);
#2031=LINE('',#13882,#2490);
#2032=LINE('',#13888,#2491);
#2033=LINE('',#13898,#2492);
#2034=LINE('',#13908,#2493);
#2035=LINE('',#13918,#2494);
#2036=LINE('',#13928,#2495);
#2037=LINE('',#13932,#2496);
#2038=LINE('',#13936,#2497);
#2039=LINE('',#13940,#2498);
#2040=LINE('',#13944,#2499);
#2041=LINE('',#13991,#2500);
#2042=LINE('',#13992,#2501);
#2043=LINE('',#14111,#2502);
#2044=LINE('',#14112,#2503);
#2045=LINE('',#14193,#2504);
#2046=LINE('',#14346,#2505);
#2047=LINE('',#14488,#2506);
#2048=LINE('',#14512,#2507);
#2049=LINE('',#14560,#2508);
#2050=LINE('',#14608,#2509);
#2051=LINE('',#14659,#2510);
#2052=LINE('',#14707,#2511);
#2053=LINE('',#14755,#2512);
#2054=LINE('',#14803,#2513);
#2055=LINE('',#14857,#2514);
#2056=LINE('',#14905,#2515);
#2057=LINE('',#14953,#2516);
#2058=LINE('',#15007,#2517);
#2059=LINE('',#15055,#2518);
#2060=LINE('',#15103,#2519);
#2061=LINE('',#15151,#2520);
#2062=LINE('',#15205,#2521);
#2063=LINE('',#15253,#2522);
#2064=LINE('',#15301,#2523);
#2065=LINE('',#15355,#2524);
#2066=LINE('',#15403,#2525);
#2067=LINE('',#15451,#2526);
#2068=LINE('',#15505,#2527);
#2069=LINE('',#15553,#2528);
#2070=LINE('',#15601,#2529);
#2071=LINE('',#15649,#2530);
#2072=LINE('',#15703,#2531);
#2073=LINE('',#15751,#2532);
#2074=LINE('',#15799,#2533);
#2075=LINE('',#15853,#2534);
#2076=LINE('',#15901,#2535);
#2077=LINE('',#15949,#2536);
#2078=LINE('',#15975,#2537);
#2079=LINE('',#15999,#2538);
#2080=LINE('',#16023,#2539);
#2081=LINE('',#16048,#2540);
#2082=LINE('',#16073,#2541);
#2083=LINE('',#16097,#2542);
#2084=LINE('',#16122,#2543);
#2085=LINE('',#16147,#2544);
#2086=LINE('',#16171,#2545);
#2087=LINE('',#16195,#2546);
#2088=LINE('',#16220,#2547);
#2089=LINE('',#16245,#2548);
#2090=LINE('',#16269,#2549);
#2091=LINE('',#16294,#2550);
#2092=LINE('',#16319,#2551);
#2093=LINE('',#16343,#2552);
#2094=LINE('',#16368,#2553);
#2095=LINE('',#16393,#2554);
#2096=LINE('',#16417,#2555);
#2097=LINE('',#16441,#2556);
#2098=LINE('',#16466,#2557);
#2099=LINE('',#16491,#2558);
#2100=LINE('',#16515,#2559);
#2101=LINE('',#16540,#2560);
#2102=LINE('',#16565,#2561);
#2103=LINE('',#16589,#2562);
#2104=LINE('',#16614,#2563);
#2105=LINE('',#16638,#2564);
#2106=LINE('',#16663,#2565);
#2107=LINE('',#16864,#2566);
#2108=LINE('',#18609,#2567);
#2109=LINE('',#18611,#2568);
#2110=LINE('',#18613,#2569);
#2111=LINE('',#18614,#2570);
#2112=LINE('',#18617,#2571);
#2113=LINE('',#18619,#2572);
#2114=LINE('',#18620,#2573);
#2115=LINE('',#18623,#2574);
#2116=LINE('',#18625,#2575);
#2117=LINE('',#18626,#2576);
#2118=LINE('',#18629,#2577);
#2119=LINE('',#18631,#2578);
#2120=LINE('',#18632,#2579);
#2121=LINE('',#18635,#2580);
#2122=LINE('',#18637,#2581);
#2123=LINE('',#18638,#2582);
#2124=LINE('',#18640,#2583);
#2125=LINE('',#18641,#2584);
#2126=LINE('',#18648,#2585);
#2127=LINE('',#18656,#2586);
#2128=LINE('',#18669,#2587);
#2129=LINE('',#18716,#2588);
#2130=LINE('',#18770,#2589);
#2131=LINE('',#18818,#2590);
#2132=LINE('',#18857,#2591);
#2133=LINE('',#18878,#2592);
#2134=LINE('',#18903,#2593);
#2135=LINE('',#18928,#2594);
#2136=LINE('',#18953,#2595);
#2137=LINE('',#19526,#2596);
#2138=LINE('',#19528,#2597);
#2139=LINE('',#19530,#2598);
#2140=LINE('',#19532,#2599);
#2141=LINE('',#19534,#2600);
#2142=LINE('',#19535,#2601);
#2143=LINE('',#19540,#2602);
#2144=LINE('',#19541,#2603);
#2145=LINE('',#19542,#2604);
#2146=LINE('',#19545,#2605);
#2147=LINE('',#19546,#2606);
#2148=LINE('',#19549,#2607);
#2149=LINE('',#19550,#2608);
#2150=LINE('',#19553,#2609);
#2151=LINE('',#19554,#2610);
#2152=LINE('',#19557,#2611);
#2153=LINE('',#19558,#2612);
#2154=LINE('',#19560,#2613);
#2155=LINE('',#19575,#2614);
#2156=LINE('',#19581,#2615);
#2157=VECTOR('',#7777,0.17);
#2158=VECTOR('',#7784,0.17);
#2159=VECTOR('',#7791,0.41);
#2160=VECTOR('',#7796,1.);
#2161=VECTOR('',#7797,1.);
#2162=VECTOR('',#7798,1.);
#2163=VECTOR('',#7801,1.);
#2164=VECTOR('',#7808,1.);
#2165=VECTOR('',#7809,1.);
#2166=VECTOR('',#7812,1.);
#2167=VECTOR('',#7813,1.);
#2168=VECTOR('',#7814,1.);
#2169=VECTOR('',#7817,1.);
#2170=VECTOR('',#7818,1.);
#2171=VECTOR('',#7819,1.);
#2172=VECTOR('',#7820,1.);
#2173=VECTOR('',#7827,1.);
#2174=VECTOR('',#7836,1.);
#2175=VECTOR('',#7837,1.);
#2176=VECTOR('',#7840,1.);
#2177=VECTOR('',#7841,1.);
#2178=VECTOR('',#7842,1.);
#2179=VECTOR('',#7843,1.);
#2180=VECTOR('',#7846,1.);
#2181=VECTOR('',#7847,1.);
#2182=VECTOR('',#7848,1.);
#2183=VECTOR('',#7851,1.);
#2184=VECTOR('',#7852,1.);
#2185=VECTOR('',#7853,1.);
#2186=VECTOR('',#7856,1.);
#2187=VECTOR('',#7857,1.);
#2188=VECTOR('',#7858,1.);
#2189=VECTOR('',#7863,1.);
#2190=VECTOR('',#7870,1.);
#2191=VECTOR('',#7875,1.);
#2192=VECTOR('',#7878,1.);
#2193=VECTOR('',#7879,1.);
#2194=VECTOR('',#7880,1.);
#2195=VECTOR('',#7881,1.);
#2196=VECTOR('',#7882,1.);
#2197=VECTOR('',#7885,1.);
#2198=VECTOR('',#7886,1.);
#2199=VECTOR('',#7903,1.1);
#2200=VECTOR('',#7906,1.);
#2201=VECTOR('',#7907,1.);
#2202=VECTOR('',#7910,1.);
#2203=VECTOR('',#7911,1.);
#2204=VECTOR('',#7912,1.);
#2205=VECTOR('',#7913,1.);
#2206=VECTOR('',#7914,1.);
#2207=VECTOR('',#7917,1.);
#2208=VECTOR('',#7924,1.);
#2209=VECTOR('',#7925,1.);
#2210=VECTOR('',#7928,1.);
#2211=VECTOR('',#7929,1.);
#2212=VECTOR('',#7932,1.);
#2213=VECTOR('',#7935,1.);
#2214=VECTOR('',#7940,1.);
#2215=VECTOR('',#7945,1.);
#2216=VECTOR('',#7948,1.);
#2217=VECTOR('',#7957,0.17);
#2218=VECTOR('',#7964,0.17);
#2219=VECTOR('',#7971,0.41);
#2220=VECTOR('',#7976,1.);
#2221=VECTOR('',#7977,1.);
#2222=VECTOR('',#7978,1.);
#2223=VECTOR('',#7979,1.);
#2224=VECTOR('',#7982,1.);
#2225=VECTOR('',#7983,1.);
#2226=VECTOR('',#7984,1.);
#2227=VECTOR('',#7985,1.);
#2228=VECTOR('',#7992,1.);
#2229=VECTOR('',#7999,1.);
#2230=VECTOR('',#8008,1.);
#2231=VECTOR('',#8009,1.);
#2232=VECTOR('',#8012,1.);
#2233=VECTOR('',#8013,1.);
#2234=VECTOR('',#8014,1.);
#2235=VECTOR('',#8015,1.);
#2236=VECTOR('',#8018,1.);
#2237=VECTOR('',#8019,1.);
#2238=VECTOR('',#8022,1.);
#2239=VECTOR('',#8023,1.);
#2240=VECTOR('',#8024,1.);
#2241=VECTOR('',#8027,1.);
#2242=VECTOR('',#8028,1.);
#2243=VECTOR('',#8029,1.);
#2244=VECTOR('',#8034,1.);
#2245=VECTOR('',#8041,1.);
#2246=VECTOR('',#8046,1.);
#2247=VECTOR('',#8049,1.);
#2248=VECTOR('',#8050,1.);
#2249=VECTOR('',#8051,1.);
#2250=VECTOR('',#8052,1.);
#2251=VECTOR('',#8053,1.);
#2252=VECTOR('',#8056,1.);
#2253=VECTOR('',#8057,1.);
#2254=VECTOR('',#8074,1.1);
#2255=VECTOR('',#8077,1.);
#2256=VECTOR('',#8078,1.);
#2257=VECTOR('',#8081,1.);
#2258=VECTOR('',#8082,1.);
#2259=VECTOR('',#8083,1.);
#2260=VECTOR('',#8084,1.);
#2261=VECTOR('',#8085,1.);
#2262=VECTOR('',#8088,1.);
#2263=VECTOR('',#8095,1.);
#2264=VECTOR('',#8096,1.);
#2265=VECTOR('',#8099,1.);
#2266=VECTOR('',#8100,1.);
#2267=VECTOR('',#8103,1.);
#2268=VECTOR('',#8106,1.);
#2269=VECTOR('',#8111,1.);
#2270=VECTOR('',#8116,1.);
#2271=VECTOR('',#8119,1.);
#2272=VECTOR('',#8128,0.3);
#2273=VECTOR('',#8143,0.4);
#2274=VECTOR('',#8152,0.6);
#2275=VECTOR('',#8159,0.4);
#2276=VECTOR('',#8166,1.);
#2277=VECTOR('',#8167,1.);
#2278=VECTOR('',#8168,1.);
#2279=VECTOR('',#8169,1.);
#2280=VECTOR('',#8172,1.);
#2281=VECTOR('',#8173,1.);
#2282=VECTOR('',#8174,1.);
#2283=VECTOR('',#8175,1.);
#2284=VECTOR('',#8198,1.);
#2285=VECTOR('',#8199,1.);
#2286=VECTOR('',#8210,0.15);
#2287=VECTOR('',#8217,0.15);
#2288=VECTOR('',#8222,0.15);
#2289=VECTOR('',#8227,0.15);
#2290=VECTOR('',#8234,0.3);
#2291=VECTOR('',#8245,0.3);
#2292=VECTOR('',#8254,0.17);
#2293=VECTOR('',#8259,0.17);
#2294=VECTOR('',#8264,1.);
#2295=VECTOR('',#8265,1.);
#2296=VECTOR('',#8266,1.);
#2297=VECTOR('',#8267,1.);
#2298=VECTOR('',#8270,1.);
#2299=VECTOR('',#8271,1.);
#2300=VECTOR('',#8272,1.);
#2301=VECTOR('',#8273,1.);
#2302=VECTOR('',#8276,1.);
#2303=VECTOR('',#8277,1.);
#2304=VECTOR('',#8278,1.);
#2305=VECTOR('',#8279,1.);
#2306=VECTOR('',#8282,1.);
#2307=VECTOR('',#8283,1.);
#2308=VECTOR('',#8284,1.);
#2309=VECTOR('',#8285,1.);
#2310=VECTOR('',#8288,1.);
#2311=VECTOR('',#8289,1.);
#2312=VECTOR('',#8290,1.);
#2313=VECTOR('',#8291,1.);
#2314=VECTOR('',#8294,1.);
#2315=VECTOR('',#8295,1.);
#2316=VECTOR('',#8296,1.);
#2317=VECTOR('',#8297,1.);
#2318=VECTOR('',#8300,1.);
#2319=VECTOR('',#8301,1.);
#2320=VECTOR('',#8302,1.);
#2321=VECTOR('',#8303,1.);
#2322=VECTOR('',#8314,1.);
#2323=VECTOR('',#8315,1.);
#2324=VECTOR('',#8318,1.);
#2325=VECTOR('',#8319,1.);
#2326=VECTOR('',#8322,1.);
#2327=VECTOR('',#8323,1.);
#2328=VECTOR('',#8326,1.);
#2329=VECTOR('',#8327,1.);
#2330=VECTOR('',#8328,1.);
#2331=VECTOR('',#8331,1.);
#2332=VECTOR('',#8332,1.);
#2333=VECTOR('',#8333,1.);
#2334=VECTOR('',#8336,1.);
#2335=VECTOR('',#8337,1.);
#2336=VECTOR('',#8340,1.);
#2337=VECTOR('',#8341,1.);
#2338=VECTOR('',#8342,1.);
#2339=VECTOR('',#8345,1.);
#2340=VECTOR('',#8346,1.);
#2341=VECTOR('',#8347,1.);
#2342=VECTOR('',#8350,1.);
#2343=VECTOR('',#8351,1.);
#2344=VECTOR('',#8354,1.);
#2345=VECTOR('',#8355,1.);
#2346=VECTOR('',#8356,1.);
#2347=VECTOR('',#8359,1.);
#2348=VECTOR('',#8360,1.);
#2349=VECTOR('',#8361,1.);
#2350=VECTOR('',#8362,1.);
#2351=VECTOR('',#8363,1.);
#2352=VECTOR('',#8364,1.);
#2353=VECTOR('',#8365,1.);
#2354=VECTOR('',#8366,1.);
#2355=VECTOR('',#8367,1.);
#2356=VECTOR('',#8368,1.);
#2357=VECTOR('',#8369,1.);
#2358=VECTOR('',#8374,0.4);
#2359=VECTOR('',#8377,0.4);
#2360=VECTOR('',#8380,1.);
#2361=VECTOR('',#8387,1.);
#2362=VECTOR('',#8390,1.);
#2363=VECTOR('',#8397,1.);
#2364=VECTOR('',#8402,1.);
#2365=VECTOR('',#8435,1.);
#2366=VECTOR('',#8464,1.);
#2367=VECTOR('',#8465,1.);
#2368=VECTOR('',#8476,1.);
#2369=VECTOR('',#8477,1.);
#2370=VECTOR('',#8488,1.);
#2371=VECTOR('',#8489,1.);
#2372=VECTOR('',#8500,0.15);
#2373=VECTOR('',#8507,0.15);
#2374=VECTOR('',#8512,0.15);
#2375=VECTOR('',#8517,0.15);
#2376=VECTOR('',#8522,1.);
#2377=VECTOR('',#8523,1.);
#2378=VECTOR('',#8524,1.);
#2379=VECTOR('',#8525,1.);
#2380=VECTOR('',#8528,1.);
#2381=VECTOR('',#8529,1.);
#2382=VECTOR('',#8530,1.);
#2383=VECTOR('',#8533,1.);
#2384=VECTOR('',#8534,1.);
#2385=VECTOR('',#8535,1.);
#2386=VECTOR('',#8538,1.);
#2387=VECTOR('',#8539,1.);
#2388=VECTOR('',#8540,1.);
#2389=VECTOR('',#8543,1.);
#2390=VECTOR('',#8544,1.);
#2391=VECTOR('',#8545,1.);
#2392=VECTOR('',#8548,1.);
#2393=VECTOR('',#8549,1.);
#2394=VECTOR('',#8556,1.);
#2395=VECTOR('',#8557,1.);
#2396=VECTOR('',#8558,1.);
#2397=VECTOR('',#8559,1.);
#2398=VECTOR('',#8562,1.);
#2399=VECTOR('',#8563,1.);
#2400=VECTOR('',#8564,1.);
#2401=VECTOR('',#8567,1.);
#2402=VECTOR('',#8568,1.);
#2403=VECTOR('',#8569,1.);
#2404=VECTOR('',#8572,1.);
#2405=VECTOR('',#8573,1.);
#2406=VECTOR('',#8574,1.);
#2407=VECTOR('',#8577,1.);
#2408=VECTOR('',#8578,1.);
#2409=VECTOR('',#8579,1.);
#2410=VECTOR('',#8582,1.);
#2411=VECTOR('',#8583,1.);
#2412=VECTOR('',#8590,0.17);
#2413=VECTOR('',#8595,0.17);
#2414=VECTOR('',#8600,1.);
#2415=VECTOR('',#8601,1.);
#2416=VECTOR('',#8602,1.);
#2417=VECTOR('',#8603,1.);
#2418=VECTOR('',#8606,1.);
#2419=VECTOR('',#8607,1.);
#2420=VECTOR('',#8608,1.);
#2421=VECTOR('',#8609,1.);
#2422=VECTOR('',#8612,1.);
#2423=VECTOR('',#8613,1.);
#2424=VECTOR('',#8614,1.);
#2425=VECTOR('',#8615,1.);
#2426=VECTOR('',#8618,1.);
#2427=VECTOR('',#8619,1.);
#2428=VECTOR('',#8620,1.);
#2429=VECTOR('',#8621,1.);
#2430=VECTOR('',#8624,1.);
#2431=VECTOR('',#8625,1.);
#2432=VECTOR('',#8626,1.);
#2433=VECTOR('',#8627,1.);
#2434=VECTOR('',#8630,1.);
#2435=VECTOR('',#8631,1.);
#2436=VECTOR('',#8632,1.);
#2437=VECTOR('',#8633,1.);
#2438=VECTOR('',#8636,1.);
#2439=VECTOR('',#8637,1.);
#2440=VECTOR('',#8638,1.);
#2441=VECTOR('',#8639,1.);
#2442=VECTOR('',#8650,1.);
#2443=VECTOR('',#8651,1.);
#2444=VECTOR('',#8654,1.);
#2445=VECTOR('',#8655,1.);
#2446=VECTOR('',#8658,1.);
#2447=VECTOR('',#8659,1.);
#2448=VECTOR('',#8662,1.);
#2449=VECTOR('',#8663,1.);
#2450=VECTOR('',#8664,1.);
#2451=VECTOR('',#8667,1.);
#2452=VECTOR('',#8668,1.);
#2453=VECTOR('',#8669,1.);
#2454=VECTOR('',#8672,1.);
#2455=VECTOR('',#8673,1.);
#2456=VECTOR('',#8676,1.);
#2457=VECTOR('',#8677,1.);
#2458=VECTOR('',#8678,1.);
#2459=VECTOR('',#8681,1.);
#2460=VECTOR('',#8682,1.);
#2461=VECTOR('',#8683,1.);
#2462=VECTOR('',#8686,1.);
#2463=VECTOR('',#8687,1.);
#2464=VECTOR('',#8690,1.);
#2465=VECTOR('',#8691,1.);
#2466=VECTOR('',#8692,1.);
#2467=VECTOR('',#8695,1.);
#2468=VECTOR('',#8696,1.);
#2469=VECTOR('',#8697,1.);
#2470=VECTOR('',#8698,1.);
#2471=VECTOR('',#8699,1.);
#2472=VECTOR('',#8700,1.);
#2473=VECTOR('',#8701,1.);
#2474=VECTOR('',#8702,1.);
#2475=VECTOR('',#8703,1.);
#2476=VECTOR('',#8704,1.);
#2477=VECTOR('',#8705,1.);
#2478=VECTOR('',#8710,0.4);
#2479=VECTOR('',#8713,0.4);
#2480=VECTOR('',#8716,1.);
#2481=VECTOR('',#8723,1.);
#2482=VECTOR('',#8726,1.);
#2483=VECTOR('',#8733,1.);
#2484=VECTOR('',#8738,1.);
#2485=VECTOR('',#8771,1.);
#2486=VECTOR('',#8800,1.);
#2487=VECTOR('',#8801,1.);
#2488=VECTOR('',#8812,1.);
#2489=VECTOR('',#8813,1.);
#2490=VECTOR('',#8826,0.35);
#2491=VECTOR('',#8833,0.35);
#2492=VECTOR('',#8846,0.25);
#2493=VECTOR('',#8859,0.25);
#2494=VECTOR('',#8872,0.25);
#2495=VECTOR('',#8885,0.25);
#2496=VECTOR('',#8890,0.15);
#2497=VECTOR('',#8895,0.15);
#2498=VECTOR('',#8900,0.15);
#2499=VECTOR('',#8905,0.15);
#2500=VECTOR('',#8916,1.);
#2501=VECTOR('',#8917,1.);
#2502=VECTOR('',#8928,1.);
#2503=VECTOR('',#8929,1.);
#2504=VECTOR('',#8934,1.);
#2505=VECTOR('',#8939,1.);
#2506=VECTOR('',#8946,0.15);
#2507=VECTOR('',#8951,0.15);
#2508=VECTOR('',#8954,0.15);
#2509=VECTOR('',#8957,0.15);
#2510=VECTOR('',#8960,0.15);
#2511=VECTOR('',#8963,0.15);
#2512=VECTOR('',#8966,0.15);
#2513=VECTOR('',#8969,0.15);
#2514=VECTOR('',#8972,0.15);
#2515=VECTOR('',#8975,0.15);
#2516=VECTOR('',#8978,0.15);
#2517=VECTOR('',#8981,0.15);
#2518=VECTOR('',#8984,0.15);
#2519=VECTOR('',#8987,0.15);
#2520=VECTOR('',#8990,0.15);
#2521=VECTOR('',#8993,0.15);
#2522=VECTOR('',#8996,0.15);
#2523=VECTOR('',#8999,0.15);
#2524=VECTOR('',#9002,0.15);
#2525=VECTOR('',#9005,0.15);
#2526=VECTOR('',#9008,0.15);
#2527=VECTOR('',#9011,0.15);
#2528=VECTOR('',#9014,0.15);
#2529=VECTOR('',#9017,0.15);
#2530=VECTOR('',#9020,0.15);
#2531=VECTOR('',#9023,0.15);
#2532=VECTOR('',#9026,0.15);
#2533=VECTOR('',#9029,0.15);
#2534=VECTOR('',#9032,0.15);
#2535=VECTOR('',#9035,0.15);
#2536=VECTOR('',#9038,0.117775);
#2537=VECTOR('',#9043,0.117775);
#2538=VECTOR('',#9046,0.117775);
#2539=VECTOR('',#9049,0.117775);
#2540=VECTOR('',#9052,0.117775);
#2541=VECTOR('',#9055,0.117775);
#2542=VECTOR('',#9058,0.117775);
#2543=VECTOR('',#9061,0.117775);
#2544=VECTOR('',#9064,0.117775);
#2545=VECTOR('',#9067,0.117775);
#2546=VECTOR('',#9070,0.117775);
#2547=VECTOR('',#9073,0.117775);
#2548=VECTOR('',#9076,0.117775);
#2549=VECTOR('',#9079,0.117775);
#2550=VECTOR('',#9082,0.117775);
#2551=VECTOR('',#9085,0.117775);
#2552=VECTOR('',#9088,0.117775);
#2553=VECTOR('',#9091,0.117775);
#2554=VECTOR('',#9094,0.117775);
#2555=VECTOR('',#9097,0.117775);
#2556=VECTOR('',#9100,0.117775);
#2557=VECTOR('',#9103,0.117775);
#2558=VECTOR('',#9106,0.117775);
#2559=VECTOR('',#9109,0.117775);
#2560=VECTOR('',#9112,0.117775);
#2561=VECTOR('',#9115,0.117775);
#2562=VECTOR('',#9118,0.117775);
#2563=VECTOR('',#9121,0.117775);
#2564=VECTOR('',#9124,0.117775);
#2565=VECTOR('',#9127,0.117775);
#2566=VECTOR('',#9132,0.1);
#2567=VECTOR('',#9143,1.);
#2568=VECTOR('',#9144,1.);
#2569=VECTOR('',#9145,1.);
#2570=VECTOR('',#9146,1.);
#2571=VECTOR('',#9149,1.);
#2572=VECTOR('',#9150,1.);
#2573=VECTOR('',#9151,1.);
#2574=VECTOR('',#9154,1.);
#2575=VECTOR('',#9155,1.);
#2576=VECTOR('',#9156,1.);
#2577=VECTOR('',#9159,1.);
#2578=VECTOR('',#9160,1.);
#2579=VECTOR('',#9161,1.);
#2580=VECTOR('',#9164,1.);
#2581=VECTOR('',#9165,1.);
#2582=VECTOR('',#9166,1.);
#2583=VECTOR('',#9169,1.);
#2584=VECTOR('',#9170,1.);
#2585=VECTOR('',#9179,0.275);
#2586=VECTOR('',#9190,0.15);
#2587=VECTOR('',#9195,0.15);
#2588=VECTOR('',#9200,0.15);
#2589=VECTOR('',#9203,0.15);
#2590=VECTOR('',#9206,0.15);
#2591=VECTOR('',#9211,0.1543);
#2592=VECTOR('',#9216,0.1543);
#2593=VECTOR('',#9219,0.1543);
#2594=VECTOR('',#9222,0.1543);
#2595=VECTOR('',#9225,0.1543);
#2596=VECTOR('',#9232,1.);
#2597=VECTOR('',#9233,1.);
#2598=VECTOR('',#9234,1.);
#2599=VECTOR('',#9235,1.);
#2600=VECTOR('',#9236,1.);
#2601=VECTOR('',#9237,1.);
#2602=VECTOR('',#9242,1.);
#2603=VECTOR('',#9243,1.);
#2604=VECTOR('',#9244,1.);
#2605=VECTOR('',#9247,1.);
#2606=VECTOR('',#9248,1.);
#2607=VECTOR('',#9251,1.);
#2608=VECTOR('',#9252,1.);
#2609=VECTOR('',#9255,1.);
#2610=VECTOR('',#9256,1.);
#2611=VECTOR('',#9259,1.);
#2612=VECTOR('',#9260,1.);
#2613=VECTOR('',#9263,1.);
#2614=VECTOR('',#9288,0.41);
#2615=VECTOR('',#9295,0.6);
#2616=CIRCLE('',#7227,0.17);
#2617=CIRCLE('',#7228,0.17);
#2618=CIRCLE('',#7230,0.17);
#2619=CIRCLE('',#7231,0.17);
#2620=CIRCLE('',#7233,0.41);
#2621=CIRCLE('',#7234,0.41);
#2622=CIRCLE('',#7237,3.48832599394285);
#2623=CIRCLE('',#7238,3.08832599394285);
#2624=CIRCLE('',#7243,0.2);
#2625=CIRCLE('',#7244,0.2);
#2626=CIRCLE('',#7246,6.99668559332711);
#2627=CIRCLE('',#7247,6.99668559332711);
#2628=CIRCLE('',#7254,1.4);
#2629=CIRCLE('',#7255,1.4);
#2630=CIRCLE('',#7257,1.4);
#2631=CIRCLE('',#7258,1.4);
#2632=CIRCLE('',#7260,1.7);
#2633=CIRCLE('',#7261,1.7);
#2634=CIRCLE('',#7262,1.2);
#2635=CIRCLE('',#7264,1.2);
#2636=CIRCLE('',#7265,0.1);
#2637=CIRCLE('',#7266,1.1);
#2638=CIRCLE('',#7268,1.1);
#2639=CIRCLE('',#7269,1.1);
#2640=CIRCLE('',#7271,1.7);
#2641=CIRCLE('',#7272,1.7);
#2642=CIRCLE('',#7274,0.1);
#2643=CIRCLE('',#7287,0.17);
#2644=CIRCLE('',#7288,0.17);
#2645=CIRCLE('',#7290,0.17);
#2646=CIRCLE('',#7291,0.17);
#2647=CIRCLE('',#7293,0.41);
#2648=CIRCLE('',#7294,0.41);
#2649=CIRCLE('',#7298,2.9940843367589);
#2650=CIRCLE('',#7299,2.9940843367589);
#2651=CIRCLE('',#7301,0.3);
#2652=CIRCLE('',#7302,0.3);
#2653=CIRCLE('',#7304,7.11398555645532);
#2654=CIRCLE('',#7305,7.11398555645532);
#2655=CIRCLE('',#7312,1.4);
#2656=CIRCLE('',#7313,1.4);
#2657=CIRCLE('',#7315,1.4);
#2658=CIRCLE('',#7316,1.4);
#2659=CIRCLE('',#7318,1.7);
#2660=CIRCLE('',#7319,1.7);
#2661=CIRCLE('',#7320,1.2);
#2662=CIRCLE('',#7322,1.2);
#2663=CIRCLE('',#7323,0.1);
#2664=CIRCLE('',#7324,1.1);
#2665=CIRCLE('',#7326,1.1);
#2666=CIRCLE('',#7327,1.1);
#2667=CIRCLE('',#7329,1.7);
#2668=CIRCLE('',#7330,1.7);
#2669=CIRCLE('',#7332,0.1);
#2670=CIRCLE('',#7345,0.3);
#2671=CIRCLE('',#7346,0.3);
#2672=CIRCLE('',#7348,0.4);
#2673=CIRCLE('',#7350,0.4);
#2674=CIRCLE('',#7352,0.4);
#2675=CIRCLE('',#7354,0.6);
#2676=CIRCLE('',#7355,0.4);
#2677=CIRCLE('',#7357,0.6);
#2678=CIRCLE('',#7365,0.6);
#2679=CIRCLE('',#7366,0.3);
#2680=CIRCLE('',#7368,0.3);
#2681=CIRCLE('',#7370,0.6);
#2682=CIRCLE('',#7375,0.15);
#2683=CIRCLE('',#7376,0.15);
#2684=CIRCLE('',#7377,0.4);
#2685=CIRCLE('',#7379,0.15);
#2686=CIRCLE('',#7380,0.15);
#2687=CIRCLE('',#7382,0.15);
#2688=CIRCLE('',#7384,0.15);
#2689=CIRCLE('',#7386,0.15);
#2690=CIRCLE('',#7387,0.15);
#2691=CIRCLE('',#7389,0.3);
#2692=CIRCLE('',#7390,0.3);
#2693=CIRCLE('',#7392,0.17);
#2694=CIRCLE('',#7394,0.3);
#2695=CIRCLE('',#7395,0.3);
#2696=CIRCLE('',#7397,0.17);
#2697=CIRCLE('',#7399,0.17);
#2698=CIRCLE('',#7401,0.17);
#2699=CIRCLE('',#7410,0.4);
#2700=CIRCLE('',#7412,0.4);
#2701=CIRCLE('',#7425,0.4);
#2702=CIRCLE('',#7428,0.1);
#2703=CIRCLE('',#7435,0.0999999999999999);
#2704=CIRCLE('',#7437,0.0999999999999999);
#2705=CIRCLE('',#7439,0.0999999999999999);
#2706=CIRCLE('',#7440,0.1);
#2707=CIRCLE('',#7442,0.0999999999999998);
#2708=CIRCLE('',#7443,0.0999999999999998);
#2709=CIRCLE('',#7444,0.0999999999999997);
#2710=CIRCLE('',#7446,0.0999999999999998);
#2711=CIRCLE('',#7447,0.0999999999999998);
#2712=CIRCLE('',#7450,0.0999999999999999);
#2713=CIRCLE('',#7451,0.1);
#2714=CIRCLE('',#7455,0.3);
#2715=CIRCLE('',#7456,0.3);
#2716=CIRCLE('',#7457,0.3);
#2717=CIRCLE('',#7459,0.3);
#2718=CIRCLE('',#7460,0.3);
#2719=CIRCLE('',#7461,0.3);
#2720=CIRCLE('',#7463,0.3);
#2721=CIRCLE('',#7464,0.3);
#2722=CIRCLE('',#7465,0.3);
#2723=CIRCLE('',#7468,0.3);
#2724=CIRCLE('',#7469,0.3);
#2725=CIRCLE('',#7470,0.3);
#2726=CIRCLE('',#7477,0.15);
#2727=CIRCLE('',#7478,0.15);
#2728=CIRCLE('',#7479,0.4);
#2729=CIRCLE('',#7481,0.15);
#2730=CIRCLE('',#7482,0.15);
#2731=CIRCLE('',#7484,0.15);
#2732=CIRCLE('',#7486,0.15);
#2733=CIRCLE('',#7488,0.15);
#2734=CIRCLE('',#7489,0.15);
#2735=CIRCLE('',#7497,0.17);
#2736=CIRCLE('',#7505,0.17);
#2737=CIRCLE('',#7507,0.17);
#2738=CIRCLE('',#7509,0.17);
#2739=CIRCLE('',#7518,0.4);
#2740=CIRCLE('',#7520,0.4);
#2741=CIRCLE('',#7533,0.4);
#2742=CIRCLE('',#7536,0.1);
#2743=CIRCLE('',#7543,0.0999999999999999);
#2744=CIRCLE('',#7545,0.0999999999999999);
#2745=CIRCLE('',#7547,0.0999999999999999);
#2746=CIRCLE('',#7548,0.1);
#2747=CIRCLE('',#7550,0.0999999999999998);
#2748=CIRCLE('',#7551,0.0999999999999998);
#2749=CIRCLE('',#7552,0.0999999999999997);
#2750=CIRCLE('',#7554,0.0999999999999998);
#2751=CIRCLE('',#7555,0.0999999999999998);
#2752=CIRCLE('',#7558,0.0999999999999999);
#2753=CIRCLE('',#7559,0.1);
#2754=CIRCLE('',#7563,0.3);
#2755=CIRCLE('',#7564,0.3);
#2756=CIRCLE('',#7565,0.3);
#2757=CIRCLE('',#7567,0.3);
#2758=CIRCLE('',#7568,0.3);
#2759=CIRCLE('',#7569,0.3);
#2760=CIRCLE('',#7571,0.3);
#2761=CIRCLE('',#7572,0.3);
#2762=CIRCLE('',#7573,0.3);
#2763=CIRCLE('',#7576,0.3);
#2764=CIRCLE('',#7577,0.3);
#2765=CIRCLE('',#7578,0.3);
#2766=CIRCLE('',#7585,0.35);
#2767=CIRCLE('',#7586,0.35);
#2768=CIRCLE('',#7588,0.35);
#2769=CIRCLE('',#7589,0.35);
#2770=CIRCLE('',#7591,0.25);
#2771=CIRCLE('',#7592,0.15);
#2772=CIRCLE('',#7594,0.25);
#2773=CIRCLE('',#7597,0.25);
#2774=CIRCLE('',#7598,0.15);
#2775=CIRCLE('',#7600,0.25);
#2776=CIRCLE('',#7603,0.25);
#2777=CIRCLE('',#7604,0.15);
#2778=CIRCLE('',#7606,0.25);
#2779=CIRCLE('',#7609,0.25);
#2780=CIRCLE('',#7610,0.15);
#2781=CIRCLE('',#7612,0.25);
#2782=CIRCLE('',#7615,0.15);
#2783=CIRCLE('',#7617,0.15);
#2784=CIRCLE('',#7619,0.15);
#2785=CIRCLE('',#7621,0.15);
#2786=CIRCLE('',#7622,0.0800000000000001);
#2787=CIRCLE('',#7623,0.0800000000000001);
#2788=CIRCLE('',#7625,0.0800000000000001);
#2789=CIRCLE('',#7626,0.0800000000000001);
#2790=CIRCLE('',#7627,0.0800000000000001);
#2791=CIRCLE('',#7628,0.0800000000000003);
#2792=CIRCLE('',#7630,0.0800000000000001);
#2793=CIRCLE('',#7631,0.0800000000000003);
#2794=CIRCLE('',#7638,0.14635);
#2795=CIRCLE('',#7669,0.117775);
#2796=CIRCLE('',#7700,0.14635);
#2797=CIRCLE('',#7701,0.05);
#2798=CIRCLE('',#7703,0.117775);
#2799=CIRCLE('',#7713,0.275);
#2800=CIRCLE('',#7715,0.275);
#2801=CIRCLE('',#7720,0.12645);
#2802=CIRCLE('',#7722,0.12645);
#2803=CIRCLE('',#7726,0.12645);
#2804=CIRCLE('',#7728,0.1543);
#2805=CIRCLE('',#7733,0.1543);
#2806=CIRCLE('',#7754,0.41);
#2807=CIRCLE('',#7755,0.41);
#2808=CIRCLE('',#7757,0.6);
#2809=CIRCLE('',#7758,0.6);
#2810=VERTEX_POINT('',#9321);
#2811=VERTEX_POINT('',#9323);
#2812=VERTEX_POINT('',#9327);
#2813=VERTEX_POINT('',#9329);
#2814=VERTEX_POINT('',#9333);
#2815=VERTEX_POINT('',#9335);
#2816=VERTEX_POINT('',#9339);
#2817=VERTEX_POINT('',#9340);
#2818=VERTEX_POINT('',#9342);
#2819=VERTEX_POINT('',#9346);
#2820=VERTEX_POINT('',#9347);
#2821=VERTEX_POINT('',#9352);
#2822=VERTEX_POINT('',#9356);
#2823=VERTEX_POINT('',#9357);
#2824=VERTEX_POINT('',#9362);
#2825=VERTEX_POINT('',#9363);
#2826=VERTEX_POINT('',#9365);
#2827=VERTEX_POINT('',#9367);
#2828=VERTEX_POINT('',#9371);
#2829=VERTEX_POINT('',#9373);
#2830=VERTEX_POINT('',#9380);
#2831=VERTEX_POINT('',#9384);
#2832=VERTEX_POINT('',#9386);
#2833=VERTEX_POINT('',#9388);
#2834=VERTEX_POINT('',#9392);
#2835=VERTEX_POINT('',#9394);
#2836=VERTEX_POINT('',#9398);
#2837=VERTEX_POINT('',#9399);
#2838=VERTEX_POINT('',#9404);
#2839=VERTEX_POINT('',#9405);
#2840=VERTEX_POINT('',#9410);
#2841=VERTEX_POINT('',#9412);
#2842=VERTEX_POINT('',#9416);
#2843=VERTEX_POINT('',#9418);
#2844=VERTEX_POINT('',#9422);
#2845=VERTEX_POINT('',#9424);
#2846=VERTEX_POINT('',#9426);
#2847=VERTEX_POINT('',#9428);
#2848=VERTEX_POINT('',#9430);
#2849=VERTEX_POINT('',#9432);
#2850=VERTEX_POINT('',#9434);
#2851=VERTEX_POINT('',#9436);
#2852=VERTEX_POINT('',#9438);
#2853=VERTEX_POINT('',#9441);
#2854=VERTEX_POINT('',#9444);
#2855=VERTEX_POINT('',#9446);
#2856=VERTEX_POINT('',#9450);
#2857=VERTEX_POINT('',#9451);
#2858=VERTEX_POINT('',#9456);
#2859=VERTEX_POINT('',#9458);
#2860=VERTEX_POINT('',#9460);
#2861=VERTEX_POINT('',#9462);
#2862=VERTEX_POINT('',#9464);
#2863=VERTEX_POINT('',#9466);
#2864=VERTEX_POINT('',#9468);
#2865=VERTEX_POINT('',#9470);
#2866=VERTEX_POINT('',#9472);
#2867=VERTEX_POINT('',#9498);
#2868=VERTEX_POINT('',#9500);
#2869=VERTEX_POINT('',#9504);
#2870=VERTEX_POINT('',#9506);
#2871=VERTEX_POINT('',#9510);
#2872=VERTEX_POINT('',#9512);
#2873=VERTEX_POINT('',#9516);
#2874=VERTEX_POINT('',#9517);
#2875=VERTEX_POINT('',#9519);
#2876=VERTEX_POINT('',#9521);
#2877=VERTEX_POINT('',#9525);
#2878=VERTEX_POINT('',#9526);
#2879=VERTEX_POINT('',#9528);
#2880=VERTEX_POINT('',#9530);
#2881=VERTEX_POINT('',#9534);
#2882=VERTEX_POINT('',#9536);
#2883=VERTEX_POINT('',#9540);
#2884=VERTEX_POINT('',#9542);
#2885=VERTEX_POINT('',#9549);
#2886=VERTEX_POINT('',#9553);
#2887=VERTEX_POINT('',#9555);
#2888=VERTEX_POINT('',#9557);
#2889=VERTEX_POINT('',#9561);
#2890=VERTEX_POINT('',#9565);
#2891=VERTEX_POINT('',#9566);
#2892=VERTEX_POINT('',#9571);
#2893=VERTEX_POINT('',#9572);
#2894=VERTEX_POINT('',#9577);
#2895=VERTEX_POINT('',#9579);
#2896=VERTEX_POINT('',#9583);
#2897=VERTEX_POINT('',#9585);
#2898=VERTEX_POINT('',#9589);
#2899=VERTEX_POINT('',#9591);
#2900=VERTEX_POINT('',#9593);
#2901=VERTEX_POINT('',#9595);
#2902=VERTEX_POINT('',#9597);
#2903=VERTEX_POINT('',#9599);
#2904=VERTEX_POINT('',#9601);
#2905=VERTEX_POINT('',#9603);
#2906=VERTEX_POINT('',#9605);
#2907=VERTEX_POINT('',#9608);
#2908=VERTEX_POINT('',#9611);
#2909=VERTEX_POINT('',#9613);
#2910=VERTEX_POINT('',#9617);
#2911=VERTEX_POINT('',#9618);
#2912=VERTEX_POINT('',#9623);
#2913=VERTEX_POINT('',#9625);
#2914=VERTEX_POINT('',#9627);
#2915=VERTEX_POINT('',#9629);
#2916=VERTEX_POINT('',#9631);
#2917=VERTEX_POINT('',#9633);
#2918=VERTEX_POINT('',#9635);
#2919=VERTEX_POINT('',#9637);
#2920=VERTEX_POINT('',#9639);
#2921=VERTEX_POINT('',#9665);
#2922=VERTEX_POINT('',#9667);
#2923=VERTEX_POINT('',#9671);
#2924=VERTEX_POINT('',#9674);
#2925=VERTEX_POINT('',#9677);
#2926=VERTEX_POINT('',#9681);
#2927=VERTEX_POINT('',#9683);
#2928=VERTEX_POINT('',#9686);
#2929=VERTEX_POINT('',#9695);
#2930=VERTEX_POINT('',#9696);
#2931=VERTEX_POINT('',#9698);
#2932=VERTEX_POINT('',#9700);
#2933=VERTEX_POINT('',#9704);
#2934=VERTEX_POINT('',#9705);
#2935=VERTEX_POINT('',#9707);
#2936=VERTEX_POINT('',#9709);
#2937=VERTEX_POINT('',#9723);
#2938=VERTEX_POINT('',#9724);
#2939=VERTEX_POINT('',#9729);
#2940=VERTEX_POINT('',#9731);
#2941=VERTEX_POINT('',#9736);
#2942=VERTEX_POINT('',#9756);
#2943=VERTEX_POINT('',#9761);
#2944=VERTEX_POINT('',#9763);
#2945=VERTEX_POINT('',#9787);
#2946=VERTEX_POINT('',#9789);
#2947=VERTEX_POINT('',#9791);
#2948=VERTEX_POINT('',#9794);
#2949=VERTEX_POINT('',#9796);
#2950=VERTEX_POINT('',#9800);
#2951=VERTEX_POINT('',#9804);
#2952=VERTEX_POINT('',#9808);
#2953=VERTEX_POINT('',#9810);
#2954=VERTEX_POINT('',#9814);
#2955=VERTEX_POINT('',#9816);
#2956=VERTEX_POINT('',#9820);
#2957=VERTEX_POINT('',#9823);
#2958=VERTEX_POINT('',#9825);
#2959=VERTEX_POINT('',#9829);
#2960=VERTEX_POINT('',#9832);
#2961=VERTEX_POINT('',#9836);
#2962=VERTEX_POINT('',#9840);
#2963=VERTEX_POINT('',#9841);
#2964=VERTEX_POINT('',#9843);
#2965=VERTEX_POINT('',#9845);
#2966=VERTEX_POINT('',#9849);
#2967=VERTEX_POINT('',#9850);
#2968=VERTEX_POINT('',#9852);
#2969=VERTEX_POINT('',#9854);
#2970=VERTEX_POINT('',#9858);
#2971=VERTEX_POINT('',#9859);
#2972=VERTEX_POINT('',#9861);
#2973=VERTEX_POINT('',#9863);
#2974=VERTEX_POINT('',#9867);
#2975=VERTEX_POINT('',#9868);
#2976=VERTEX_POINT('',#9870);
#2977=VERTEX_POINT('',#9872);
#2978=VERTEX_POINT('',#9876);
#2979=VERTEX_POINT('',#9877);
#2980=VERTEX_POINT('',#9879);
#2981=VERTEX_POINT('',#9881);
#2982=VERTEX_POINT('',#9885);
#2983=VERTEX_POINT('',#9886);
#2984=VERTEX_POINT('',#9888);
#2985=VERTEX_POINT('',#9890);
#2986=VERTEX_POINT('',#9894);
#2987=VERTEX_POINT('',#9895);
#2988=VERTEX_POINT('',#9897);
#2989=VERTEX_POINT('',#9899);
#2990=VERTEX_POINT('',#9903);
#2991=VERTEX_POINT('',#9906);
#2992=VERTEX_POINT('',#9918);
#2993=VERTEX_POINT('',#9920);
#2994=VERTEX_POINT('',#9924);
#2995=VERTEX_POINT('',#9926);
#2996=VERTEX_POINT('',#9930);
#2997=VERTEX_POINT('',#9931);
#2998=VERTEX_POINT('',#9933);
#2999=VERTEX_POINT('',#9940);
#3000=VERTEX_POINT('',#9969);
#3001=VERTEX_POINT('',#9971);
#3002=VERTEX_POINT('',#10007);
#3003=VERTEX_POINT('',#10009);
#3004=VERTEX_POINT('',#10016);
#3005=VERTEX_POINT('',#10045);
#3006=VERTEX_POINT('',#10047);
#3007=VERTEX_POINT('',#10076);
#3008=VERTEX_POINT('',#10085);
#3009=VERTEX_POINT('',#10087);
#3010=VERTEX_POINT('',#10094);
#3011=VERTEX_POINT('',#10123);
#3012=VERTEX_POINT('',#10125);
#3013=VERTEX_POINT('',#10154);
#3014=VERTEX_POINT('',#10163);
#3015=VERTEX_POINT('',#10165);
#3016=VERTEX_POINT('',#10200);
#3017=VERTEX_POINT('',#10229);
#3018=VERTEX_POINT('',#10238);
#3019=VERTEX_POINT('',#10240);
#3020=VERTEX_POINT('',#10245);
#3021=VERTEX_POINT('',#10247);
#3022=VERTEX_POINT('',#10262);
#3023=VERTEX_POINT('',#10274);
#3024=VERTEX_POINT('',#10280);
#3025=VERTEX_POINT('',#10282);
#3026=VERTEX_POINT('',#10315);
#3027=VERTEX_POINT('',#10317);
#3028=VERTEX_POINT('',#10355);
#3029=VERTEX_POINT('',#10360);
#3030=VERTEX_POINT('',#10404);
#3031=VERTEX_POINT('',#10406);
#3032=VERTEX_POINT('',#10450);
#3033=VERTEX_POINT('',#10455);
#3034=VERTEX_POINT('',#10494);
#3035=VERTEX_POINT('',#10523);
#3036=VERTEX_POINT('',#10529);
#3037=VERTEX_POINT('',#10535);
#3038=VERTEX_POINT('',#10547);
#3039=VERTEX_POINT('',#10548);
#3040=VERTEX_POINT('',#10553);
#3041=VERTEX_POINT('',#10588);
#3042=VERTEX_POINT('',#10590);
#3043=VERTEX_POINT('',#10625);
#3044=VERTEX_POINT('',#10632);
#3045=VERTEX_POINT('',#10638);
#3046=VERTEX_POINT('',#10645);
#3047=VERTEX_POINT('',#10652);
#3048=VERTEX_POINT('',#10681);
#3049=VERTEX_POINT('',#10747);
#3050=VERTEX_POINT('',#10800);
#3051=VERTEX_POINT('',#10812);
#3052=VERTEX_POINT('',#10874);
#3053=VERTEX_POINT('',#10884);
#3054=VERTEX_POINT('',#10891);
#3055=VERTEX_POINT('',#10920);
#3056=VERTEX_POINT('',#10922);
#3057=VERTEX_POINT('',#11047);
#3058=VERTEX_POINT('',#11082);
#3059=VERTEX_POINT('',#11198);
#3060=VERTEX_POINT('',#11205);
#3061=VERTEX_POINT('',#11234);
#3062=VERTEX_POINT('',#11236);
#3063=VERTEX_POINT('',#11287);
#3064=VERTEX_POINT('',#11316);
#3065=VERTEX_POINT('',#11323);
#3066=VERTEX_POINT('',#11345);
#3067=VERTEX_POINT('',#11380);
#3068=VERTEX_POINT('',#11408);
#3069=VERTEX_POINT('',#11511);
#3070=VERTEX_POINT('',#11512);
#3071=VERTEX_POINT('',#11514);
#3072=VERTEX_POINT('',#11518);
#3073=VERTEX_POINT('',#11519);
#3074=VERTEX_POINT('',#11521);
#3075=VERTEX_POINT('',#11525);
#3076=VERTEX_POINT('',#11526);
#3077=VERTEX_POINT('',#11528);
#3078=VERTEX_POINT('',#11563);
#3079=VERTEX_POINT('',#11564);
#3080=VERTEX_POINT('',#11566);
#3081=VERTEX_POINT('',#11771);
#3082=VERTEX_POINT('',#11772);
#3083=VERTEX_POINT('',#11777);
#3084=VERTEX_POINT('',#11779);
#3085=VERTEX_POINT('',#11784);
#3086=VERTEX_POINT('',#11804);
#3087=VERTEX_POINT('',#11809);
#3088=VERTEX_POINT('',#11811);
#3089=VERTEX_POINT('',#11835);
#3090=VERTEX_POINT('',#11837);
#3091=VERTEX_POINT('',#11839);
#3092=VERTEX_POINT('',#11842);
#3093=VERTEX_POINT('',#11844);
#3094=VERTEX_POINT('',#11848);
#3095=VERTEX_POINT('',#11852);
#3096=VERTEX_POINT('',#11856);
#3097=VERTEX_POINT('',#11858);
#3098=VERTEX_POINT('',#11862);
#3099=VERTEX_POINT('',#11863);
#3100=VERTEX_POINT('',#11865);
#3101=VERTEX_POINT('',#11867);
#3102=VERTEX_POINT('',#11871);
#3103=VERTEX_POINT('',#11873);
#3104=VERTEX_POINT('',#11877);
#3105=VERTEX_POINT('',#11879);
#3106=VERTEX_POINT('',#11883);
#3107=VERTEX_POINT('',#11885);
#3108=VERTEX_POINT('',#11889);
#3109=VERTEX_POINT('',#11891);
#3110=VERTEX_POINT('',#11898);
#3111=VERTEX_POINT('',#11901);
#3112=VERTEX_POINT('',#11902);
#3113=VERTEX_POINT('',#11904);
#3114=VERTEX_POINT('',#11906);
#3115=VERTEX_POINT('',#11910);
#3116=VERTEX_POINT('',#11912);
#3117=VERTEX_POINT('',#11916);
#3118=VERTEX_POINT('',#11918);
#3119=VERTEX_POINT('',#11922);
#3120=VERTEX_POINT('',#11924);
#3121=VERTEX_POINT('',#11928);
#3122=VERTEX_POINT('',#11930);
#3123=VERTEX_POINT('',#11937);
#3124=VERTEX_POINT('',#11940);
#3125=VERTEX_POINT('',#11944);
#3126=VERTEX_POINT('',#11948);
#3127=VERTEX_POINT('',#11949);
#3128=VERTEX_POINT('',#11951);
#3129=VERTEX_POINT('',#11953);
#3130=VERTEX_POINT('',#11957);
#3131=VERTEX_POINT('',#11958);
#3132=VERTEX_POINT('',#11960);
#3133=VERTEX_POINT('',#11962);
#3134=VERTEX_POINT('',#11966);
#3135=VERTEX_POINT('',#11967);
#3136=VERTEX_POINT('',#11969);
#3137=VERTEX_POINT('',#11971);
#3138=VERTEX_POINT('',#11975);
#3139=VERTEX_POINT('',#11976);
#3140=VERTEX_POINT('',#11978);
#3141=VERTEX_POINT('',#11980);
#3142=VERTEX_POINT('',#11984);
#3143=VERTEX_POINT('',#11985);
#3144=VERTEX_POINT('',#11987);
#3145=VERTEX_POINT('',#11989);
#3146=VERTEX_POINT('',#11993);
#3147=VERTEX_POINT('',#11994);
#3148=VERTEX_POINT('',#11996);
#3149=VERTEX_POINT('',#11998);
#3150=VERTEX_POINT('',#12002);
#3151=VERTEX_POINT('',#12003);
#3152=VERTEX_POINT('',#12005);
#3153=VERTEX_POINT('',#12007);
#3154=VERTEX_POINT('',#12011);
#3155=VERTEX_POINT('',#12014);
#3156=VERTEX_POINT('',#12026);
#3157=VERTEX_POINT('',#12028);
#3158=VERTEX_POINT('',#12032);
#3159=VERTEX_POINT('',#12034);
#3160=VERTEX_POINT('',#12038);
#3161=VERTEX_POINT('',#12039);
#3162=VERTEX_POINT('',#12041);
#3163=VERTEX_POINT('',#12048);
#3164=VERTEX_POINT('',#12077);
#3165=VERTEX_POINT('',#12079);
#3166=VERTEX_POINT('',#12115);
#3167=VERTEX_POINT('',#12117);
#3168=VERTEX_POINT('',#12124);
#3169=VERTEX_POINT('',#12153);
#3170=VERTEX_POINT('',#12155);
#3171=VERTEX_POINT('',#12184);
#3172=VERTEX_POINT('',#12193);
#3173=VERTEX_POINT('',#12195);
#3174=VERTEX_POINT('',#12202);
#3175=VERTEX_POINT('',#12231);
#3176=VERTEX_POINT('',#12233);
#3177=VERTEX_POINT('',#12262);
#3178=VERTEX_POINT('',#12271);
#3179=VERTEX_POINT('',#12273);
#3180=VERTEX_POINT('',#12308);
#3181=VERTEX_POINT('',#12337);
#3182=VERTEX_POINT('',#12346);
#3183=VERTEX_POINT('',#12348);
#3184=VERTEX_POINT('',#12353);
#3185=VERTEX_POINT('',#12355);
#3186=VERTEX_POINT('',#12370);
#3187=VERTEX_POINT('',#12382);
#3188=VERTEX_POINT('',#12388);
#3189=VERTEX_POINT('',#12390);
#3190=VERTEX_POINT('',#12423);
#3191=VERTEX_POINT('',#12425);
#3192=VERTEX_POINT('',#12463);
#3193=VERTEX_POINT('',#12468);
#3194=VERTEX_POINT('',#12512);
#3195=VERTEX_POINT('',#12514);
#3196=VERTEX_POINT('',#12558);
#3197=VERTEX_POINT('',#12563);
#3198=VERTEX_POINT('',#12602);
#3199=VERTEX_POINT('',#12631);
#3200=VERTEX_POINT('',#12637);
#3201=VERTEX_POINT('',#12643);
#3202=VERTEX_POINT('',#12655);
#3203=VERTEX_POINT('',#12656);
#3204=VERTEX_POINT('',#12661);
#3205=VERTEX_POINT('',#12696);
#3206=VERTEX_POINT('',#12698);
#3207=VERTEX_POINT('',#12733);
#3208=VERTEX_POINT('',#12740);
#3209=VERTEX_POINT('',#12746);
#3210=VERTEX_POINT('',#12753);
#3211=VERTEX_POINT('',#12760);
#3212=VERTEX_POINT('',#12789);
#3213=VERTEX_POINT('',#12855);
#3214=VERTEX_POINT('',#12908);
#3215=VERTEX_POINT('',#12920);
#3216=VERTEX_POINT('',#12982);
#3217=VERTEX_POINT('',#12992);
#3218=VERTEX_POINT('',#12999);
#3219=VERTEX_POINT('',#13028);
#3220=VERTEX_POINT('',#13030);
#3221=VERTEX_POINT('',#13155);
#3222=VERTEX_POINT('',#13190);
#3223=VERTEX_POINT('',#13306);
#3224=VERTEX_POINT('',#13313);
#3225=VERTEX_POINT('',#13342);
#3226=VERTEX_POINT('',#13344);
#3227=VERTEX_POINT('',#13395);
#3228=VERTEX_POINT('',#13424);
#3229=VERTEX_POINT('',#13431);
#3230=VERTEX_POINT('',#13453);
#3231=VERTEX_POINT('',#13488);
#3232=VERTEX_POINT('',#13516);
#3233=VERTEX_POINT('',#13619);
#3234=VERTEX_POINT('',#13620);
#3235=VERTEX_POINT('',#13622);
#3236=VERTEX_POINT('',#13626);
#3237=VERTEX_POINT('',#13627);
#3238=VERTEX_POINT('',#13629);
#3239=VERTEX_POINT('',#13633);
#3240=VERTEX_POINT('',#13634);
#3241=VERTEX_POINT('',#13636);
#3242=VERTEX_POINT('',#13671);
#3243=VERTEX_POINT('',#13672);
#3244=VERTEX_POINT('',#13674);
#3245=VERTEX_POINT('',#13879);
#3246=VERTEX_POINT('',#13881);
#3247=VERTEX_POINT('',#13885);
#3248=VERTEX_POINT('',#13887);
#3249=VERTEX_POINT('',#13891);
#3250=VERTEX_POINT('',#13893);
#3251=VERTEX_POINT('',#13896);
#3252=VERTEX_POINT('',#13901);
#3253=VERTEX_POINT('',#13903);
#3254=VERTEX_POINT('',#13906);
#3255=VERTEX_POINT('',#13911);
#3256=VERTEX_POINT('',#13913);
#3257=VERTEX_POINT('',#13916);
#3258=VERTEX_POINT('',#13921);
#3259=VERTEX_POINT('',#13923);
#3260=VERTEX_POINT('',#13926);
#3261=VERTEX_POINT('',#13931);
#3262=VERTEX_POINT('',#13935);
#3263=VERTEX_POINT('',#13939);
#3264=VERTEX_POINT('',#13943);
#3265=VERTEX_POINT('',#13971);
#3266=VERTEX_POINT('',#13972);
#3267=VERTEX_POINT('',#13974);
#3268=VERTEX_POINT('',#13980);
#3269=VERTEX_POINT('',#13988);
#3270=VERTEX_POINT('',#13989);
#3271=VERTEX_POINT('',#14018);
#3272=VERTEX_POINT('',#14019);
#3273=VERTEX_POINT('',#14056);
#3274=VERTEX_POINT('',#14057);
#3275=VERTEX_POINT('',#14094);
#3276=VERTEX_POINT('',#14095);
#3277=VERTEX_POINT('',#14108);
#3278=VERTEX_POINT('',#14109);
#3279=VERTEX_POINT('',#14138);
#3280=VERTEX_POINT('',#14139);
#3281=VERTEX_POINT('',#14187);
#3282=VERTEX_POINT('',#14192);
#3283=VERTEX_POINT('',#14218);
#3284=VERTEX_POINT('',#14267);
#3285=VERTEX_POINT('',#14300);
#3286=VERTEX_POINT('',#14341);
#3287=VERTEX_POINT('',#14367);
#3288=VERTEX_POINT('',#14424);
#3289=VERTEX_POINT('',#14486);
#3290=VERTEX_POINT('',#14487);
#3291=VERTEX_POINT('',#14489);
#3292=VERTEX_POINT('',#14500);
#3293=VERTEX_POINT('',#14510);
#3294=VERTEX_POINT('',#14511);
#3295=VERTEX_POINT('',#14558);
#3296=VERTEX_POINT('',#14559);
#3297=VERTEX_POINT('',#14606);
#3298=VERTEX_POINT('',#14607);
#3299=VERTEX_POINT('',#14657);
#3300=VERTEX_POINT('',#14658);
#3301=VERTEX_POINT('',#14705);
#3302=VERTEX_POINT('',#14706);
#3303=VERTEX_POINT('',#14753);
#3304=VERTEX_POINT('',#14754);
#3305=VERTEX_POINT('',#14801);
#3306=VERTEX_POINT('',#14802);
#3307=VERTEX_POINT('',#14855);
#3308=VERTEX_POINT('',#14856);
#3309=VERTEX_POINT('',#14903);
#3310=VERTEX_POINT('',#14904);
#3311=VERTEX_POINT('',#14951);
#3312=VERTEX_POINT('',#14952);
#3313=VERTEX_POINT('',#15005);
#3314=VERTEX_POINT('',#15006);
#3315=VERTEX_POINT('',#15053);
#3316=VERTEX_POINT('',#15054);
#3317=VERTEX_POINT('',#15101);
#3318=VERTEX_POINT('',#15102);
#3319=VERTEX_POINT('',#15149);
#3320=VERTEX_POINT('',#15150);
#3321=VERTEX_POINT('',#15203);
#3322=VERTEX_POINT('',#15204);
#3323=VERTEX_POINT('',#15251);
#3324=VERTEX_POINT('',#15252);
#3325=VERTEX_POINT('',#15299);
#3326=VERTEX_POINT('',#15300);
#3327=VERTEX_POINT('',#15353);
#3328=VERTEX_POINT('',#15354);
#3329=VERTEX_POINT('',#15401);
#3330=VERTEX_POINT('',#15402);
#3331=VERTEX_POINT('',#15449);
#3332=VERTEX_POINT('',#15450);
#3333=VERTEX_POINT('',#15503);
#3334=VERTEX_POINT('',#15504);
#3335=VERTEX_POINT('',#15551);
#3336=VERTEX_POINT('',#15552);
#3337=VERTEX_POINT('',#15599);
#3338=VERTEX_POINT('',#15600);
#3339=VERTEX_POINT('',#15647);
#3340=VERTEX_POINT('',#15648);
#3341=VERTEX_POINT('',#15701);
#3342=VERTEX_POINT('',#15702);
#3343=VERTEX_POINT('',#15749);
#3344=VERTEX_POINT('',#15750);
#3345=VERTEX_POINT('',#15797);
#3346=VERTEX_POINT('',#15798);
#3347=VERTEX_POINT('',#15851);
#3348=VERTEX_POINT('',#15852);
#3349=VERTEX_POINT('',#15899);
#3350=VERTEX_POINT('',#15900);
#3351=VERTEX_POINT('',#15947);
#3352=VERTEX_POINT('',#15948);
#3353=VERTEX_POINT('',#15950);
#3354=VERTEX_POINT('',#15961);
#3355=VERTEX_POINT('',#15973);
#3356=VERTEX_POINT('',#15974);
#3357=VERTEX_POINT('',#15997);
#3358=VERTEX_POINT('',#15998);
#3359=VERTEX_POINT('',#16021);
#3360=VERTEX_POINT('',#16022);
#3361=VERTEX_POINT('',#16046);
#3362=VERTEX_POINT('',#16047);
#3363=VERTEX_POINT('',#16071);
#3364=VERTEX_POINT('',#16072);
#3365=VERTEX_POINT('',#16095);
#3366=VERTEX_POINT('',#16096);
#3367=VERTEX_POINT('',#16120);
#3368=VERTEX_POINT('',#16121);
#3369=VERTEX_POINT('',#16145);
#3370=VERTEX_POINT('',#16146);
#3371=VERTEX_POINT('',#16169);
#3372=VERTEX_POINT('',#16170);
#3373=VERTEX_POINT('',#16193);
#3374=VERTEX_POINT('',#16194);
#3375=VERTEX_POINT('',#16218);
#3376=VERTEX_POINT('',#16219);
#3377=VERTEX_POINT('',#16243);
#3378=VERTEX_POINT('',#16244);
#3379=VERTEX_POINT('',#16267);
#3380=VERTEX_POINT('',#16268);
#3381=VERTEX_POINT('',#16292);
#3382=VERTEX_POINT('',#16293);
#3383=VERTEX_POINT('',#16317);
#3384=VERTEX_POINT('',#16318);
#3385=VERTEX_POINT('',#16341);
#3386=VERTEX_POINT('',#16342);
#3387=VERTEX_POINT('',#16366);
#3388=VERTEX_POINT('',#16367);
#3389=VERTEX_POINT('',#16391);
#3390=VERTEX_POINT('',#16392);
#3391=VERTEX_POINT('',#16415);
#3392=VERTEX_POINT('',#16416);
#3393=VERTEX_POINT('',#16439);
#3394=VERTEX_POINT('',#16440);
#3395=VERTEX_POINT('',#16464);
#3396=VERTEX_POINT('',#16465);
#3397=VERTEX_POINT('',#16489);
#3398=VERTEX_POINT('',#16490);
#3399=VERTEX_POINT('',#16513);
#3400=VERTEX_POINT('',#16514);
#3401=VERTEX_POINT('',#16538);
#3402=VERTEX_POINT('',#16539);
#3403=VERTEX_POINT('',#16563);
#3404=VERTEX_POINT('',#16564);
#3405=VERTEX_POINT('',#16587);
#3406=VERTEX_POINT('',#16588);
#3407=VERTEX_POINT('',#16612);
#3408=VERTEX_POINT('',#16613);
#3409=VERTEX_POINT('',#16636);
#3410=VERTEX_POINT('',#16637);
#3411=VERTEX_POINT('',#16661);
#3412=VERTEX_POINT('',#16662);
#3413=VERTEX_POINT('',#16685);
#3414=VERTEX_POINT('',#16807);
#3415=VERTEX_POINT('',#16845);
#3416=VERTEX_POINT('',#16863);
#3417=VERTEX_POINT('',#17650);
#3418=VERTEX_POINT('',#17728);
#3419=VERTEX_POINT('',#18607);
#3420=VERTEX_POINT('',#18608);
#3421=VERTEX_POINT('',#18610);
#3422=VERTEX_POINT('',#18612);
#3423=VERTEX_POINT('',#18616);
#3424=VERTEX_POINT('',#18618);
#3425=VERTEX_POINT('',#18622);
#3426=VERTEX_POINT('',#18624);
#3427=VERTEX_POINT('',#18628);
#3428=VERTEX_POINT('',#18630);
#3429=VERTEX_POINT('',#18634);
#3430=VERTEX_POINT('',#18636);
#3431=VERTEX_POINT('',#18644);
#3432=VERTEX_POINT('',#18647);
#3433=VERTEX_POINT('',#18654);
#3434=VERTEX_POINT('',#18655);
#3435=VERTEX_POINT('',#18657);
#3436=VERTEX_POINT('',#18667);
#3437=VERTEX_POINT('',#18668);
#3438=VERTEX_POINT('',#18670);
#3439=VERTEX_POINT('',#18714);
#3440=VERTEX_POINT('',#18715);
#3441=VERTEX_POINT('',#18768);
#3442=VERTEX_POINT('',#18769);
#3443=VERTEX_POINT('',#18816);
#3444=VERTEX_POINT('',#18817);
#3445=VERTEX_POINT('',#18819);
#3446=VERTEX_POINT('',#18833);
#3447=VERTEX_POINT('',#18855);
#3448=VERTEX_POINT('',#18856);
#3449=VERTEX_POINT('',#18858);
#3450=VERTEX_POINT('',#18866);
#3451=VERTEX_POINT('',#18876);
#3452=VERTEX_POINT('',#18877);
#3453=VERTEX_POINT('',#18901);
#3454=VERTEX_POINT('',#18902);
#3455=VERTEX_POINT('',#18926);
#3456=VERTEX_POINT('',#18927);
#3457=VERTEX_POINT('',#18951);
#3458=VERTEX_POINT('',#18952);
#3459=VERTEX_POINT('',#18954);
#3460=VERTEX_POINT('',#18960);
#3461=VERTEX_POINT('',#19524);
#3462=VERTEX_POINT('',#19525);
#3463=VERTEX_POINT('',#19527);
#3464=VERTEX_POINT('',#19529);
#3465=VERTEX_POINT('',#19531);
#3466=VERTEX_POINT('',#19533);
#3467=VERTEX_POINT('',#19538);
#3468=VERTEX_POINT('',#19539);
#3469=VERTEX_POINT('',#19544);
#3470=VERTEX_POINT('',#19548);
#3471=VERTEX_POINT('',#19552);
#3472=VERTEX_POINT('',#19556);
#3473=VERTEX_POINT('',#19572);
#3474=VERTEX_POINT('',#19574);
#3475=VERTEX_POINT('',#19578);
#3476=VERTEX_POINT('',#19580);
#3477=EDGE_CURVE('',#2810,#2810,#2616,.T.);
#3478=EDGE_CURVE('',#2810,#2811,#1698,.T.);
#3479=EDGE_CURVE('',#2811,#2811,#2617,.T.);
#3480=EDGE_CURVE('',#2812,#2812,#2618,.T.);
#3481=EDGE_CURVE('',#2812,#2813,#1699,.T.);
#3482=EDGE_CURVE('',#2813,#2813,#2619,.T.);
#3483=EDGE_CURVE('',#2814,#2814,#2620,.T.);
#3484=EDGE_CURVE('',#2814,#2815,#1700,.T.);
#3485=EDGE_CURVE('',#2815,#2815,#2621,.T.);
#3486=EDGE_CURVE('',#2816,#2817,#1701,.T.);
#3487=EDGE_CURVE('',#2818,#2816,#1702,.T.);
#3488=EDGE_CURVE('',#2818,#2817,#1703,.T.);
#3489=EDGE_CURVE('',#2819,#2820,#1704,.T.);
#3490=EDGE_CURVE('',#2819,#2818,#2622,.T.);
#3491=EDGE_CURVE('',#2820,#2816,#2623,.T.);
#3492=EDGE_CURVE('',#2821,#2820,#1705,.T.);
#3493=EDGE_CURVE('',#2819,#2821,#1706,.T.);
#3494=EDGE_CURVE('',#2822,#2823,#1707,.T.);
#3495=EDGE_CURVE('',#2817,#2822,#1708,.T.);
#3496=EDGE_CURVE('',#2823,#2818,#1709,.T.);
#3497=EDGE_CURVE('',#2824,#2825,#1710,.T.);
#3498=EDGE_CURVE('',#2824,#2826,#1711,.T.);
#3499=EDGE_CURVE('',#2827,#2826,#1712,.T.);
#3500=EDGE_CURVE('',#2825,#2827,#1713,.T.);
#3501=EDGE_CURVE('',#2828,#2819,#2624,.T.);
#3502=EDGE_CURVE('',#2829,#2821,#2625,.T.);
#3503=EDGE_CURVE('',#2828,#2829,#1714,.T.);
#3504=EDGE_CURVE('',#2824,#2828,#2626,.T.);
#3505=EDGE_CURVE('',#2826,#2829,#2627,.T.);
#3506=EDGE_CURVE('',#2830,#2822,#1715,.T.);
#3507=EDGE_CURVE('',#2827,#2830,#1716,.T.);
#3508=EDGE_CURVE('',#2830,#2831,#1717,.T.);
#3509=EDGE_CURVE('',#2832,#2831,#1718,.T.);
#3510=EDGE_CURVE('',#2833,#2832,#1719,.T.);
#3511=EDGE_CURVE('',#2825,#2833,#1720,.T.);
#3512=EDGE_CURVE('',#2834,#2823,#1721,.T.);
#3513=EDGE_CURVE('',#2834,#2835,#1722,.T.);
#3514=EDGE_CURVE('',#2831,#2835,#1723,.T.);
#3515=EDGE_CURVE('',#2836,#2837,#1724,.T.);
#3516=EDGE_CURVE('',#2835,#2836,#1725,.T.);
#3517=EDGE_CURVE('',#2837,#2834,#1726,.T.);
#3518=EDGE_CURVE('',#2838,#2839,#1727,.T.);
#3519=EDGE_CURVE('',#2833,#2838,#1728,.T.);
#3520=EDGE_CURVE('',#2839,#2832,#1729,.T.);
#3521=EDGE_CURVE('',#2837,#2840,#2628,.T.);
#3522=EDGE_CURVE('',#2840,#2841,#1730,.T.);
#3523=EDGE_CURVE('',#2836,#2841,#2629,.T.);
#3524=EDGE_CURVE('',#2842,#2839,#2630,.T.);
#3525=EDGE_CURVE('',#2842,#2843,#1731,.T.);
#3526=EDGE_CURVE('',#2843,#2838,#2631,.T.);
#3527=EDGE_CURVE('',#2841,#2844,#1732,.T.);
#3528=EDGE_CURVE('',#2844,#2845,#2632,.T.);
#3529=EDGE_CURVE('',#2845,#2846,#1733,.T.);
#3530=EDGE_CURVE('',#2846,#2847,#1734,.T.);
#3531=EDGE_CURVE('',#2847,#2848,#1735,.T.);
#3532=EDGE_CURVE('',#2848,#2849,#1736,.T.);
#3533=EDGE_CURVE('',#2849,#2850,#1737,.T.);
#3534=EDGE_CURVE('',#2850,#2851,#2633,.T.);
#3535=EDGE_CURVE('',#2851,#2852,#1738,.T.);
#3536=EDGE_CURVE('',#2852,#2842,#1739,.T.);
#3537=EDGE_CURVE('',#2853,#2853,#2634,.T.);
#3538=EDGE_CURVE('',#2854,#2854,#2635,.T.);
#3539=EDGE_CURVE('',#2854,#2855,#2636,.T.);
#3540=EDGE_CURVE('',#2855,#2855,#2637,.T.);
#3541=EDGE_CURVE('',#2856,#2857,#2638,.T.);
#3542=EDGE_CURVE('',#2857,#2856,#2639,.T.);
#3543=EDGE_CURVE('',#2857,#2855,#1740,.T.);
#3544=EDGE_CURVE('',#2858,#2843,#1741,.T.);
#3545=EDGE_CURVE('',#2859,#2858,#1742,.T.);
#3546=EDGE_CURVE('',#2860,#2859,#2640,.T.);
#3547=EDGE_CURVE('',#2861,#2860,#1743,.T.);
#3548=EDGE_CURVE('',#2862,#2861,#1744,.T.);
#3549=EDGE_CURVE('',#2863,#2862,#1745,.T.);
#3550=EDGE_CURVE('',#2864,#2863,#1746,.T.);
#3551=EDGE_CURVE('',#2865,#2864,#1747,.T.);
#3552=EDGE_CURVE('',#2866,#2865,#2641,.T.);
#3553=EDGE_CURVE('',#2840,#2866,#1748,.T.);
#3554=EDGE_CURVE('',#2853,#2856,#2642,.T.);
#3555=EDGE_CURVE('',#2851,#2859,#1749,.T.);
#3556=EDGE_CURVE('',#2860,#2850,#1750,.T.);
#3557=EDGE_CURVE('',#2866,#2844,#1751,.T.);
#3558=EDGE_CURVE('',#2845,#2865,#1752,.T.);
#3559=EDGE_CURVE('',#2864,#2846,#1753,.T.);
#3560=EDGE_CURVE('',#2861,#2849,#1754,.T.);
#3561=EDGE_CURVE('',#2858,#2852,#1755,.T.);
#3562=EDGE_CURVE('',#2862,#2848,#1756,.T.);
#3563=EDGE_CURVE('',#2863,#2847,#1757,.T.);
#3564=EDGE_CURVE('',#2867,#2867,#2643,.T.);
#3565=EDGE_CURVE('',#2867,#2868,#1758,.T.);
#3566=EDGE_CURVE('',#2868,#2868,#2644,.T.);
#3567=EDGE_CURVE('',#2869,#2869,#2645,.T.);
#3568=EDGE_CURVE('',#2869,#2870,#1759,.T.);
#3569=EDGE_CURVE('',#2870,#2870,#2646,.T.);
#3570=EDGE_CURVE('',#2871,#2871,#2647,.T.);
#3571=EDGE_CURVE('',#2871,#2872,#1760,.T.);
#3572=EDGE_CURVE('',#2872,#2872,#2648,.T.);
#3573=EDGE_CURVE('',#2873,#2874,#1761,.T.);
#3574=EDGE_CURVE('',#2875,#2874,#1762,.T.);
#3575=EDGE_CURVE('',#2876,#2875,#1763,.T.);
#3576=EDGE_CURVE('',#2873,#2876,#1764,.T.);
#3577=EDGE_CURVE('',#2877,#2878,#1765,.T.);
#3578=EDGE_CURVE('',#2877,#2879,#1766,.T.);
#3579=EDGE_CURVE('',#2880,#2879,#1767,.T.);
#3580=EDGE_CURVE('',#2878,#2880,#1768,.T.);
#3581=EDGE_CURVE('',#2881,#2876,#2649,.T.);
#3582=EDGE_CURVE('',#2882,#2875,#2650,.T.);
#3583=EDGE_CURVE('',#2881,#2882,#1769,.T.);
#3584=EDGE_CURVE('',#2883,#2881,#2651,.T.);
#3585=EDGE_CURVE('',#2884,#2882,#2652,.T.);
#3586=EDGE_CURVE('',#2883,#2884,#1770,.T.);
#3587=EDGE_CURVE('',#2877,#2883,#2653,.T.);
#3588=EDGE_CURVE('',#2879,#2884,#2654,.T.);
#3589=EDGE_CURVE('',#2880,#2885,#1771,.T.);
#3590=EDGE_CURVE('',#2885,#2874,#1772,.T.);
#3591=EDGE_CURVE('',#2885,#2886,#1773,.T.);
#3592=EDGE_CURVE('',#2887,#2886,#1774,.T.);
#3593=EDGE_CURVE('',#2888,#2887,#1775,.T.);
#3594=EDGE_CURVE('',#2878,#2888,#1776,.T.);
#3595=EDGE_CURVE('',#2874,#2889,#1777,.T.);
#3596=EDGE_CURVE('',#2886,#2889,#1778,.T.);
#3597=EDGE_CURVE('',#2890,#2891,#1779,.T.);
#3598=EDGE_CURVE('',#2889,#2890,#1780,.T.);
#3599=EDGE_CURVE('',#2891,#2873,#1781,.T.);
#3600=EDGE_CURVE('',#2892,#2893,#1782,.T.);
#3601=EDGE_CURVE('',#2888,#2892,#1783,.T.);
#3602=EDGE_CURVE('',#2893,#2887,#1784,.T.);
#3603=EDGE_CURVE('',#2891,#2894,#2655,.T.);
#3604=EDGE_CURVE('',#2894,#2895,#1785,.T.);
#3605=EDGE_CURVE('',#2890,#2895,#2656,.T.);
#3606=EDGE_CURVE('',#2896,#2893,#2657,.T.);
#3607=EDGE_CURVE('',#2896,#2897,#1786,.T.);
#3608=EDGE_CURVE('',#2897,#2892,#2658,.T.);
#3609=EDGE_CURVE('',#2895,#2898,#1787,.T.);
#3610=EDGE_CURVE('',#2898,#2899,#2659,.T.);
#3611=EDGE_CURVE('',#2899,#2900,#1788,.T.);
#3612=EDGE_CURVE('',#2900,#2901,#1789,.T.);
#3613=EDGE_CURVE('',#2901,#2902,#1790,.T.);
#3614=EDGE_CURVE('',#2902,#2903,#1791,.T.);
#3615=EDGE_CURVE('',#2903,#2904,#1792,.T.);
#3616=EDGE_CURVE('',#2904,#2905,#2660,.T.);
#3617=EDGE_CURVE('',#2905,#2906,#1793,.T.);
#3618=EDGE_CURVE('',#2906,#2896,#1794,.T.);
#3619=EDGE_CURVE('',#2907,#2907,#2661,.T.);
#3620=EDGE_CURVE('',#2908,#2908,#2662,.T.);
#3621=EDGE_CURVE('',#2908,#2909,#2663,.T.);
#3622=EDGE_CURVE('',#2909,#2909,#2664,.T.);
#3623=EDGE_CURVE('',#2910,#2911,#2665,.T.);
#3624=EDGE_CURVE('',#2911,#2910,#2666,.T.);
#3625=EDGE_CURVE('',#2911,#2909,#1795,.T.);
#3626=EDGE_CURVE('',#2912,#2897,#1796,.T.);
#3627=EDGE_CURVE('',#2913,#2912,#1797,.T.);
#3628=EDGE_CURVE('',#2914,#2913,#2667,.T.);
#3629=EDGE_CURVE('',#2915,#2914,#1798,.T.);
#3630=EDGE_CURVE('',#2916,#2915,#1799,.T.);
#3631=EDGE_CURVE('',#2917,#2916,#1800,.T.);
#3632=EDGE_CURVE('',#2918,#2917,#1801,.T.);
#3633=EDGE_CURVE('',#2919,#2918,#1802,.T.);
#3634=EDGE_CURVE('',#2920,#2919,#2668,.T.);
#3635=EDGE_CURVE('',#2894,#2920,#1803,.T.);
#3636=EDGE_CURVE('',#2907,#2910,#2669,.T.);
#3637=EDGE_CURVE('',#2905,#2913,#1804,.T.);
#3638=EDGE_CURVE('',#2914,#2904,#1805,.T.);
#3639=EDGE_CURVE('',#2920,#2898,#1806,.T.);
#3640=EDGE_CURVE('',#2899,#2919,#1807,.T.);
#3641=EDGE_CURVE('',#2918,#2900,#1808,.T.);
#3642=EDGE_CURVE('',#2915,#2903,#1809,.T.);
#3643=EDGE_CURVE('',#2912,#2906,#1810,.T.);
#3644=EDGE_CURVE('',#2916,#2902,#1811,.T.);
#3645=EDGE_CURVE('',#2917,#2901,#1812,.T.);
#3646=EDGE_CURVE('',#2921,#2921,#2670,.T.);
#3647=EDGE_CURVE('',#2921,#2922,#1813,.T.);
#3648=EDGE_CURVE('',#2922,#2922,#2671,.T.);
#3649=EDGE_CURVE('',#2923,#2923,#2672,.T.);
#3650=EDGE_CURVE('',#2924,#2924,#2673,.T.);
#3651=EDGE_CURVE('',#2925,#2925,#2674,.T.);
#3652=EDGE_CURVE('',#2925,#2924,#1814,.T.);
#3653=EDGE_CURVE('',#2926,#2926,#2675,.T.);
#3654=EDGE_CURVE('',#2927,#2927,#2676,.T.);
#3655=EDGE_CURVE('',#2926,#2928,#1815,.T.);
#3656=EDGE_CURVE('',#2928,#2928,#2677,.T.);
#3657=EDGE_CURVE('',#2923,#2927,#1816,.T.);
#3658=EDGE_CURVE('',#2929,#2930,#1817,.T.);
#3659=EDGE_CURVE('',#2931,#2929,#1818,.T.);
#3660=EDGE_CURVE('',#2932,#2931,#1819,.T.);
#3661=EDGE_CURVE('',#2930,#2932,#1820,.T.);
#3662=EDGE_CURVE('',#2933,#2934,#1821,.T.);
#3663=EDGE_CURVE('',#2935,#2933,#1822,.T.);
#3664=EDGE_CURVE('',#2936,#2935,#1823,.T.);
#3665=EDGE_CURVE('',#2934,#2936,#1824,.T.);
#3666=EDGE_CURVE('',#2931,#2936,#2678,.T.);
#3667=EDGE_CURVE('',#2934,#2929,#2679,.T.);
#3668=EDGE_CURVE('',#2933,#2930,#2680,.T.);
#3669=EDGE_CURVE('',#2932,#2935,#2681,.T.);
#3670=EDGE_CURVE('',#2937,#2938,#171,.T.);
#3671=EDGE_CURVE('',#2938,#2939,#1825,.T.);
#3672=EDGE_CURVE('',#2939,#2940,#172,.T.);
#3673=EDGE_CURVE('',#2941,#2940,#173,.T.);
#3674=EDGE_CURVE('',#2941,#2942,#174,.T.);
#3675=EDGE_CURVE('',#2942,#2943,#1826,.T.);
#3676=EDGE_CURVE('',#2943,#2944,#175,.T.);
#3677=EDGE_CURVE('',#2937,#2944,#176,.T.);
#3678=EDGE_CURVE('',#2945,#2945,#2682,.T.);
#3679=EDGE_CURVE('',#2946,#2946,#2683,.T.);
#3680=EDGE_CURVE('',#2947,#2947,#2684,.T.);
#3681=EDGE_CURVE('',#2948,#2948,#2685,.T.);
#3682=EDGE_CURVE('',#2948,#2949,#1827,.T.);
#3683=EDGE_CURVE('',#2949,#2949,#2686,.T.);
#3684=EDGE_CURVE('',#2950,#2950,#2687,.T.);
#3685=EDGE_CURVE('',#2950,#2946,#1828,.T.);
#3686=EDGE_CURVE('',#2951,#2951,#2688,.T.);
#3687=EDGE_CURVE('',#2951,#2945,#1829,.T.);
#3688=EDGE_CURVE('',#2952,#2952,#2689,.T.);
#3689=EDGE_CURVE('',#2952,#2953,#1830,.T.);
#3690=EDGE_CURVE('',#2953,#2953,#2690,.T.);
#3691=EDGE_CURVE('',#2954,#2954,#2691,.T.);
#3692=EDGE_CURVE('',#2954,#2955,#1831,.T.);
#3693=EDGE_CURVE('',#2955,#2955,#2692,.T.);
#3694=EDGE_CURVE('',#2956,#2956,#2693,.T.);
#3695=EDGE_CURVE('',#2957,#2957,#2694,.T.);
#3696=EDGE_CURVE('',#2957,#2958,#1832,.T.);
#3697=EDGE_CURVE('',#2958,#2958,#2695,.T.);
#3698=EDGE_CURVE('',#2959,#2959,#2696,.T.);
#3699=EDGE_CURVE('',#2956,#2960,#1833,.T.);
#3700=EDGE_CURVE('',#2960,#2960,#2697,.T.);
#3701=EDGE_CURVE('',#2959,#2961,#1834,.T.);
#3702=EDGE_CURVE('',#2961,#2961,#2698,.T.);
#3703=EDGE_CURVE('',#2962,#2963,#1835,.T.);
#3704=EDGE_CURVE('',#2964,#2962,#1836,.T.);
#3705=EDGE_CURVE('',#2965,#2964,#1837,.T.);
#3706=EDGE_CURVE('',#2965,#2963,#1838,.T.);
#3707=EDGE_CURVE('',#2966,#2967,#1839,.T.);
#3708=EDGE_CURVE('',#2966,#2968,#1840,.T.);
#3709=EDGE_CURVE('',#2969,#2968,#1841,.T.);
#3710=EDGE_CURVE('',#2967,#2969,#1842,.T.);
#3711=EDGE_CURVE('',#2970,#2971,#1843,.T.);
#3712=EDGE_CURVE('',#2970,#2972,#1844,.T.);
#3713=EDGE_CURVE('',#2973,#2972,#1845,.T.);
#3714=EDGE_CURVE('',#2971,#2973,#1846,.T.);
#3715=EDGE_CURVE('',#2974,#2975,#1847,.T.);
#3716=EDGE_CURVE('',#2974,#2976,#1848,.T.);
#3717=EDGE_CURVE('',#2977,#2976,#1849,.T.);
#3718=EDGE_CURVE('',#2975,#2977,#1850,.T.);
#3719=EDGE_CURVE('',#2978,#2979,#1851,.T.);
#3720=EDGE_CURVE('',#2978,#2980,#1852,.T.);
#3721=EDGE_CURVE('',#2981,#2980,#1853,.T.);
#3722=EDGE_CURVE('',#2979,#2981,#1854,.T.);
#3723=EDGE_CURVE('',#2982,#2983,#1855,.T.);
#3724=EDGE_CURVE('',#2984,#2982,#1856,.T.);
#3725=EDGE_CURVE('',#2985,#2984,#1857,.T.);
#3726=EDGE_CURVE('',#2985,#2983,#1858,.T.);
#3727=EDGE_CURVE('',#2986,#2987,#1859,.T.);
#3728=EDGE_CURVE('',#2988,#2986,#1860,.T.);
#3729=EDGE_CURVE('',#2989,#2988,#1861,.T.);
#3730=EDGE_CURVE('',#2989,#2987,#1862,.T.);
#3731=EDGE_CURVE('',#2990,#2990,#2699,.T.);
#3732=EDGE_CURVE('',#2991,#2991,#2700,.T.);
#3733=EDGE_CURVE('',#2963,#2978,#1863,.T.);
#3734=EDGE_CURVE('',#2980,#2965,#1864,.T.);
#3735=EDGE_CURVE('',#2983,#2966,#1865,.T.);
#3736=EDGE_CURVE('',#2968,#2985,#1866,.T.);
#3737=EDGE_CURVE('',#2987,#2970,#1867,.T.);
#3738=EDGE_CURVE('',#2972,#2989,#1868,.T.);
#3739=EDGE_CURVE('',#2992,#2974,#1869,.T.);
#3740=EDGE_CURVE('',#2993,#2992,#1870,.T.);
#3741=EDGE_CURVE('',#2976,#2993,#1871,.T.);
#3742=EDGE_CURVE('',#2994,#2992,#1872,.T.);
#3743=EDGE_CURVE('',#2995,#2994,#1873,.T.);
#3744=EDGE_CURVE('',#2993,#2995,#1874,.T.);
#3745=EDGE_CURVE('',#2996,#2997,#1875,.T.);
#3746=EDGE_CURVE('',#2998,#2997,#177,.T.);
#3747=EDGE_CURVE('',#2999,#2998,#178,.T.);
#3748=EDGE_CURVE('',#3000,#2999,#1876,.T.);
#3749=EDGE_CURVE('',#3001,#3000,#179,.T.);
#3750=EDGE_CURVE('',#2996,#3001,#180,.T.);
#3751=EDGE_CURVE('',#2995,#3002,#1877,.T.);
#3752=EDGE_CURVE('',#3003,#3002,#181,.T.);
#3753=EDGE_CURVE('',#3004,#3003,#182,.T.);
#3754=EDGE_CURVE('',#3005,#3004,#1878,.T.);
#3755=EDGE_CURVE('',#3006,#3005,#183,.T.);
#3756=EDGE_CURVE('',#3007,#3006,#184,.T.);
#3757=EDGE_CURVE('',#3007,#2977,#1879,.T.);
#3758=EDGE_CURVE('',#2988,#3008,#1880,.T.);
#3759=EDGE_CURVE('',#3009,#3008,#185,.T.);
#3760=EDGE_CURVE('',#3010,#3009,#186,.T.);
#3761=EDGE_CURVE('',#3011,#3010,#1881,.T.);
#3762=EDGE_CURVE('',#3012,#3011,#187,.T.);
#3763=EDGE_CURVE('',#3013,#3012,#188,.T.);
#3764=EDGE_CURVE('',#3013,#2973,#1882,.T.);
#3765=EDGE_CURVE('',#2984,#3014,#1883,.T.);
#3766=EDGE_CURVE('',#3015,#3014,#189,.T.);
#3767=EDGE_CURVE('',#2943,#3015,#190,.T.);
#3768=EDGE_CURVE('',#3016,#2942,#191,.T.);
#3769=EDGE_CURVE('',#3017,#3016,#192,.T.);
#3770=EDGE_CURVE('',#3017,#2969,#1884,.T.);
#3771=EDGE_CURVE('',#3018,#2979,#1885,.T.);
#3772=EDGE_CURVE('',#3018,#3019,#193,.T.);
#3773=EDGE_CURVE('',#3019,#3020,#1886,.T.);
#3774=EDGE_CURVE('',#3020,#3021,#194,.T.);
#3775=EDGE_CURVE('',#2962,#3021,#1887,.T.);
#3776=EDGE_CURVE('',#3007,#2997,#195,.T.);
#3777=EDGE_CURVE('',#2996,#3002,#196,.T.);
#3778=EDGE_CURVE('',#3022,#2994,#1888,.T.);
#3779=EDGE_CURVE('',#3022,#3008,#197,.T.);
#3780=EDGE_CURVE('',#3023,#2986,#1889,.T.);
#3781=EDGE_CURVE('',#3023,#3014,#198,.T.);
#3782=EDGE_CURVE('',#3024,#2982,#1890,.T.);
#3783=EDGE_CURVE('',#3024,#3025,#199,.T.);
#3784=EDGE_CURVE('',#3025,#3018,#200,.T.);
#3785=EDGE_CURVE('',#2981,#3026,#1891,.T.);
#3786=EDGE_CURVE('',#3027,#3026,#201,.T.);
#3787=EDGE_CURVE('',#3027,#3028,#202,.T.);
#3788=EDGE_CURVE('',#3029,#3028,#203,.T.);
#3789=EDGE_CURVE('',#3029,#3030,#1892,.T.);
#3790=EDGE_CURVE('',#3031,#3030,#204,.T.);
#3791=EDGE_CURVE('',#3031,#3032,#205,.T.);
#3792=EDGE_CURVE('',#3033,#3032,#206,.T.);
#3793=EDGE_CURVE('',#3033,#2964,#1893,.T.);
#3794=EDGE_CURVE('',#3021,#3034,#207,.T.);
#3795=EDGE_CURVE('',#3034,#3035,#208,.T.);
#3796=EDGE_CURVE('',#2967,#3035,#1894,.T.);
#3797=EDGE_CURVE('',#3017,#3036,#209,.T.);
#3798=EDGE_CURVE('',#2971,#3036,#1895,.T.);
#3799=EDGE_CURVE('',#3013,#3037,#210,.T.);
#3800=EDGE_CURVE('',#2975,#3037,#1896,.T.);
#3801=EDGE_CURVE('',#3038,#3039,#211,.T.);
#3802=EDGE_CURVE('',#3039,#3040,#212,.T.);
#3803=EDGE_CURVE('',#3040,#3041,#1897,.T.);
#3804=EDGE_CURVE('',#3041,#3042,#213,.T.);
#3805=EDGE_CURVE('',#3042,#3043,#214,.T.);
#3806=EDGE_CURVE('',#3038,#3043,#1898,.T.);
#3807=EDGE_CURVE('',#3044,#3044,#2701,.T.);
#3808=EDGE_CURVE('',#3044,#2991,#1899,.T.);
#3809=EDGE_CURVE('',#2947,#2990,#1900,.T.);
#3810=EDGE_CURVE('',#3038,#3045,#215,.T.);
#3811=EDGE_CURVE('',#3046,#3043,#216,.T.);
#3812=EDGE_CURVE('',#3047,#3046,#217,.T.);
#3813=EDGE_CURVE('',#3048,#3047,#1901,.T.);
#3814=EDGE_CURVE('',#3045,#3048,#218,.T.);
#3815=EDGE_CURVE('',#3006,#2998,#219,.T.);
#3816=EDGE_CURVE('',#3045,#3049,#220,.T.);
#3817=EDGE_CURVE('',#3049,#3039,#221,.T.);
#3818=EDGE_CURVE('',#2999,#3005,#222,.T.);
#3819=EDGE_CURVE('',#3050,#3048,#223,.T.);
#3820=EDGE_CURVE('',#3049,#3050,#2702,.F.);
#3821=EDGE_CURVE('',#3004,#3000,#224,.T.);
#3822=EDGE_CURVE('',#3047,#3051,#225,.T.);
#3823=EDGE_CURVE('',#3051,#3050,#1902,.T.);
#3824=EDGE_CURVE('',#3001,#3003,#226,.T.);
#3825=EDGE_CURVE('',#3042,#3052,#227,.T.);
#3826=EDGE_CURVE('',#3052,#3046,#228,.T.);
#3827=EDGE_CURVE('',#3053,#3037,#229,.T.);
#3828=EDGE_CURVE('',#3054,#3053,#230,.T.);
#3829=EDGE_CURVE('',#3055,#3054,#1903,.T.);
#3830=EDGE_CURVE('',#3056,#3055,#231,.T.);
#3831=EDGE_CURVE('',#3022,#3056,#232,.T.);
#3832=EDGE_CURVE('',#3012,#3053,#233,.T.);
#3833=EDGE_CURVE('',#3054,#3011,#234,.T.);
#3834=EDGE_CURVE('',#3010,#3055,#235,.T.);
#3835=EDGE_CURVE('',#3056,#3009,#236,.T.);
#3836=EDGE_CURVE('',#3057,#3036,#237,.T.);
#3837=EDGE_CURVE('',#2939,#3057,#238,.T.);
#3838=EDGE_CURVE('',#3058,#2938,#239,.T.);
#3839=EDGE_CURVE('',#3023,#3058,#240,.T.);
#3840=EDGE_CURVE('',#3016,#3057,#241,.T.);
#3841=EDGE_CURVE('',#3058,#3015,#242,.T.);
#3842=EDGE_CURVE('',#3059,#3035,#243,.T.);
#3843=EDGE_CURVE('',#3060,#3059,#244,.T.);
#3844=EDGE_CURVE('',#3061,#3060,#1904,.T.);
#3845=EDGE_CURVE('',#3062,#3061,#245,.T.);
#3846=EDGE_CURVE('',#3024,#3062,#246,.T.);
#3847=EDGE_CURVE('',#3034,#3063,#247,.T.);
#3848=EDGE_CURVE('',#3063,#3059,#248,.T.);
#3849=EDGE_CURVE('',#3064,#3063,#2703,.F.);
#3850=EDGE_CURVE('',#3060,#3064,#249,.T.);
#3851=EDGE_CURVE('',#3064,#3065,#1905,.T.);
#3852=EDGE_CURVE('',#3065,#3061,#250,.T.);
#3853=EDGE_CURVE('',#3062,#3066,#251,.T.);
#3854=EDGE_CURVE('',#3066,#3025,#252,.T.);
#3855=EDGE_CURVE('',#3066,#3065,#2704,.F.);
#3856=EDGE_CURVE('',#3065,#3019,#2705,.F.);
#3857=EDGE_CURVE('',#3019,#3066,#2706,.F.);
#3858=EDGE_CURVE('',#3051,#3052,#2707,.F.);
#3859=EDGE_CURVE('',#3052,#3067,#2708,.F.);
#3860=EDGE_CURVE('',#3067,#3051,#2709,.F.);
#3861=EDGE_CURVE('',#3063,#3020,#2710,.F.);
#3862=EDGE_CURVE('',#3020,#3064,#2711,.F.);
#3863=EDGE_CURVE('',#3068,#3049,#2712,.F.);
#3864=EDGE_CURVE('',#3050,#3068,#2713,.F.);
#3865=EDGE_CURVE('',#3068,#3067,#1906,.T.);
#3866=EDGE_CURVE('',#3040,#3068,#253,.T.);
#3867=EDGE_CURVE('',#3067,#3041,#254,.T.);
#3868=EDGE_CURVE('',#3069,#3070,#2714,.F.);
#3869=EDGE_CURVE('',#3071,#3069,#2715,.F.);
#3870=EDGE_CURVE('',#3070,#3071,#2716,.F.);
#3871=EDGE_CURVE('',#3072,#3073,#2717,.F.);
#3872=EDGE_CURVE('',#3074,#3072,#2718,.F.);
#3873=EDGE_CURVE('',#3073,#3074,#2719,.F.);
#3874=EDGE_CURVE('',#3075,#3076,#2720,.F.);
#3875=EDGE_CURVE('',#3077,#3075,#2721,.F.);
#3876=EDGE_CURVE('',#3076,#3077,#2722,.F.);
#3877=EDGE_CURVE('',#3070,#3077,#1907,.T.);
#3878=EDGE_CURVE('',#3075,#3069,#1908,.T.);
#3879=EDGE_CURVE('',#3032,#3076,#255,.T.);
#3880=EDGE_CURVE('',#3077,#3033,#256,.T.);
#3881=EDGE_CURVE('',#3078,#3079,#2723,.F.);
#3882=EDGE_CURVE('',#3080,#3078,#2724,.F.);
#3883=EDGE_CURVE('',#3079,#3080,#2725,.F.);
#3884=EDGE_CURVE('',#3078,#3074,#1909,.T.);
#3885=EDGE_CURVE('',#3072,#3080,#1910,.T.);
#3886=EDGE_CURVE('',#3076,#3079,#257,.T.);
#3887=EDGE_CURVE('',#3080,#3075,#258,.T.);
#3888=EDGE_CURVE('',#3030,#3078,#259,.T.);
#3889=EDGE_CURVE('',#3079,#3031,#260,.T.);
#3890=EDGE_CURVE('',#3028,#3073,#261,.T.);
#3891=EDGE_CURVE('',#3074,#3029,#262,.T.);
#3892=EDGE_CURVE('',#3073,#3071,#263,.T.);
#3893=EDGE_CURVE('',#3069,#3072,#264,.T.);
#3894=EDGE_CURVE('',#3026,#3070,#265,.T.);
#3895=EDGE_CURVE('',#3071,#3027,#266,.T.);
#3896=EDGE_CURVE('',#3081,#3082,#267,.T.);
#3897=EDGE_CURVE('',#3082,#3083,#1911,.T.);
#3898=EDGE_CURVE('',#3083,#3084,#268,.T.);
#3899=EDGE_CURVE('',#3085,#3084,#269,.T.);
#3900=EDGE_CURVE('',#3085,#3086,#270,.T.);
#3901=EDGE_CURVE('',#3086,#3087,#1912,.T.);
#3902=EDGE_CURVE('',#3087,#3088,#271,.T.);
#3903=EDGE_CURVE('',#3081,#3088,#272,.T.);
#3904=EDGE_CURVE('',#3089,#3089,#2726,.T.);
#3905=EDGE_CURVE('',#3090,#3090,#2727,.T.);
#3906=EDGE_CURVE('',#3091,#3091,#2728,.T.);
#3907=EDGE_CURVE('',#3092,#3092,#2729,.T.);
#3908=EDGE_CURVE('',#3092,#3093,#1913,.T.);
#3909=EDGE_CURVE('',#3093,#3093,#2730,.T.);
#3910=EDGE_CURVE('',#3094,#3094,#2731,.T.);
#3911=EDGE_CURVE('',#3094,#3090,#1914,.T.);
#3912=EDGE_CURVE('',#3095,#3095,#2732,.T.);
#3913=EDGE_CURVE('',#3095,#3089,#1915,.T.);
#3914=EDGE_CURVE('',#3096,#3096,#2733,.T.);
#3915=EDGE_CURVE('',#3096,#3097,#1916,.T.);
#3916=EDGE_CURVE('',#3097,#3097,#2734,.T.);
#3917=EDGE_CURVE('',#3098,#3099,#1917,.T.);
#3918=EDGE_CURVE('',#3098,#3100,#1918,.T.);
#3919=EDGE_CURVE('',#3100,#3101,#1919,.T.);
#3920=EDGE_CURVE('',#3099,#3101,#1920,.T.);
#3921=EDGE_CURVE('',#3102,#3098,#1921,.T.);
#3922=EDGE_CURVE('',#3102,#3103,#1922,.T.);
#3923=EDGE_CURVE('',#3103,#3100,#1923,.T.);
#3924=EDGE_CURVE('',#3104,#3102,#1924,.T.);
#3925=EDGE_CURVE('',#3104,#3105,#1925,.T.);
#3926=EDGE_CURVE('',#3105,#3103,#1926,.T.);
#3927=EDGE_CURVE('',#3106,#3104,#1927,.T.);
#3928=EDGE_CURVE('',#3106,#3107,#1928,.T.);
#3929=EDGE_CURVE('',#3107,#3105,#1929,.T.);
#3930=EDGE_CURVE('',#3108,#3106,#1930,.T.);
#3931=EDGE_CURVE('',#3108,#3109,#1931,.T.);
#3932=EDGE_CURVE('',#3109,#3107,#1932,.T.);
#3933=EDGE_CURVE('',#3099,#3108,#1933,.T.);
#3934=EDGE_CURVE('',#3101,#3109,#1934,.T.);
#3935=EDGE_CURVE('',#3110,#3110,#2735,.T.);
#3936=EDGE_CURVE('',#3111,#3112,#1935,.T.);
#3937=EDGE_CURVE('',#3111,#3113,#1936,.T.);
#3938=EDGE_CURVE('',#3113,#3114,#1937,.T.);
#3939=EDGE_CURVE('',#3112,#3114,#1938,.T.);
#3940=EDGE_CURVE('',#3115,#3111,#1939,.T.);
#3941=EDGE_CURVE('',#3115,#3116,#1940,.T.);
#3942=EDGE_CURVE('',#3116,#3113,#1941,.T.);
#3943=EDGE_CURVE('',#3117,#3115,#1942,.T.);
#3944=EDGE_CURVE('',#3117,#3118,#1943,.T.);
#3945=EDGE_CURVE('',#3118,#3116,#1944,.T.);
#3946=EDGE_CURVE('',#3119,#3117,#1945,.T.);
#3947=EDGE_CURVE('',#3119,#3120,#1946,.T.);
#3948=EDGE_CURVE('',#3120,#3118,#1947,.T.);
#3949=EDGE_CURVE('',#3121,#3119,#1948,.T.);
#3950=EDGE_CURVE('',#3121,#3122,#1949,.T.);
#3951=EDGE_CURVE('',#3122,#3120,#1950,.T.);
#3952=EDGE_CURVE('',#3112,#3121,#1951,.T.);
#3953=EDGE_CURVE('',#3114,#3122,#1952,.T.);
#3954=EDGE_CURVE('',#3123,#3123,#2736,.T.);
#3955=EDGE_CURVE('',#3123,#3124,#1953,.T.);
#3956=EDGE_CURVE('',#3124,#3124,#2737,.T.);
#3957=EDGE_CURVE('',#3110,#3125,#1954,.T.);
#3958=EDGE_CURVE('',#3125,#3125,#2738,.T.);
#3959=EDGE_CURVE('',#3126,#3127,#1955,.T.);
#3960=EDGE_CURVE('',#3128,#3126,#1956,.T.);
#3961=EDGE_CURVE('',#3129,#3128,#1957,.T.);
#3962=EDGE_CURVE('',#3129,#3127,#1958,.T.);
#3963=EDGE_CURVE('',#3130,#3131,#1959,.T.);
#3964=EDGE_CURVE('',#3130,#3132,#1960,.T.);
#3965=EDGE_CURVE('',#3133,#3132,#1961,.T.);
#3966=EDGE_CURVE('',#3131,#3133,#1962,.T.);
#3967=EDGE_CURVE('',#3134,#3135,#1963,.T.);
#3968=EDGE_CURVE('',#3134,#3136,#1964,.T.);
#3969=EDGE_CURVE('',#3137,#3136,#1965,.T.);
#3970=EDGE_CURVE('',#3135,#3137,#1966,.T.);
#3971=EDGE_CURVE('',#3138,#3139,#1967,.T.);
#3972=EDGE_CURVE('',#3138,#3140,#1968,.T.);
#3973=EDGE_CURVE('',#3141,#3140,#1969,.T.);
#3974=EDGE_CURVE('',#3139,#3141,#1970,.T.);
#3975=EDGE_CURVE('',#3142,#3143,#1971,.T.);
#3976=EDGE_CURVE('',#3142,#3144,#1972,.T.);
#3977=EDGE_CURVE('',#3145,#3144,#1973,.T.);
#3978=EDGE_CURVE('',#3143,#3145,#1974,.T.);
#3979=EDGE_CURVE('',#3146,#3147,#1975,.T.);
#3980=EDGE_CURVE('',#3148,#3146,#1976,.T.);
#3981=EDGE_CURVE('',#3149,#3148,#1977,.T.);
#3982=EDGE_CURVE('',#3149,#3147,#1978,.T.);
#3983=EDGE_CURVE('',#3150,#3151,#1979,.T.);
#3984=EDGE_CURVE('',#3152,#3150,#1980,.T.);
#3985=EDGE_CURVE('',#3153,#3152,#1981,.T.);
#3986=EDGE_CURVE('',#3153,#3151,#1982,.T.);
#3987=EDGE_CURVE('',#3154,#3154,#2739,.T.);
#3988=EDGE_CURVE('',#3155,#3155,#2740,.T.);
#3989=EDGE_CURVE('',#3127,#3142,#1983,.T.);
#3990=EDGE_CURVE('',#3144,#3129,#1984,.T.);
#3991=EDGE_CURVE('',#3147,#3130,#1985,.T.);
#3992=EDGE_CURVE('',#3132,#3149,#1986,.T.);
#3993=EDGE_CURVE('',#3151,#3134,#1987,.T.);
#3994=EDGE_CURVE('',#3136,#3153,#1988,.T.);
#3995=EDGE_CURVE('',#3156,#3138,#1989,.T.);
#3996=EDGE_CURVE('',#3157,#3156,#1990,.T.);
#3997=EDGE_CURVE('',#3140,#3157,#1991,.T.);
#3998=EDGE_CURVE('',#3158,#3156,#1992,.T.);
#3999=EDGE_CURVE('',#3159,#3158,#1993,.T.);
#4000=EDGE_CURVE('',#3157,#3159,#1994,.T.);
#4001=EDGE_CURVE('',#3160,#3161,#1995,.T.);
#4002=EDGE_CURVE('',#3162,#3161,#273,.T.);
#4003=EDGE_CURVE('',#3163,#3162,#274,.T.);
#4004=EDGE_CURVE('',#3164,#3163,#1996,.T.);
#4005=EDGE_CURVE('',#3165,#3164,#275,.T.);
#4006=EDGE_CURVE('',#3160,#3165,#276,.T.);
#4007=EDGE_CURVE('',#3159,#3166,#1997,.T.);
#4008=EDGE_CURVE('',#3167,#3166,#277,.T.);
#4009=EDGE_CURVE('',#3168,#3167,#278,.T.);
#4010=EDGE_CURVE('',#3169,#3168,#1998,.T.);
#4011=EDGE_CURVE('',#3170,#3169,#279,.T.);
#4012=EDGE_CURVE('',#3171,#3170,#280,.T.);
#4013=EDGE_CURVE('',#3171,#3141,#1999,.T.);
#4014=EDGE_CURVE('',#3152,#3172,#2000,.T.);
#4015=EDGE_CURVE('',#3173,#3172,#281,.T.);
#4016=EDGE_CURVE('',#3174,#3173,#282,.T.);
#4017=EDGE_CURVE('',#3175,#3174,#2001,.T.);
#4018=EDGE_CURVE('',#3176,#3175,#283,.T.);
#4019=EDGE_CURVE('',#3177,#3176,#284,.T.);
#4020=EDGE_CURVE('',#3177,#3137,#2002,.T.);
#4021=EDGE_CURVE('',#3148,#3178,#2003,.T.);
#4022=EDGE_CURVE('',#3179,#3178,#285,.T.);
#4023=EDGE_CURVE('',#3087,#3179,#286,.T.);
#4024=EDGE_CURVE('',#3180,#3086,#287,.T.);
#4025=EDGE_CURVE('',#3181,#3180,#288,.T.);
#4026=EDGE_CURVE('',#3181,#3133,#2004,.T.);
#4027=EDGE_CURVE('',#3182,#3143,#2005,.T.);
#4028=EDGE_CURVE('',#3182,#3183,#289,.T.);
#4029=EDGE_CURVE('',#3183,#3184,#2006,.T.);
#4030=EDGE_CURVE('',#3184,#3185,#290,.T.);
#4031=EDGE_CURVE('',#3126,#3185,#2007,.T.);
#4032=EDGE_CURVE('',#3171,#3161,#291,.T.);
#4033=EDGE_CURVE('',#3160,#3166,#292,.T.);
#4034=EDGE_CURVE('',#3186,#3158,#2008,.T.);
#4035=EDGE_CURVE('',#3186,#3172,#293,.T.);
#4036=EDGE_CURVE('',#3187,#3150,#2009,.T.);
#4037=EDGE_CURVE('',#3187,#3178,#294,.T.);
#4038=EDGE_CURVE('',#3188,#3146,#2010,.T.);
#4039=EDGE_CURVE('',#3188,#3189,#295,.T.);
#4040=EDGE_CURVE('',#3189,#3182,#296,.T.);
#4041=EDGE_CURVE('',#3145,#3190,#2011,.T.);
#4042=EDGE_CURVE('',#3191,#3190,#297,.T.);
#4043=EDGE_CURVE('',#3191,#3192,#298,.T.);
#4044=EDGE_CURVE('',#3193,#3192,#299,.T.);
#4045=EDGE_CURVE('',#3193,#3194,#2012,.T.);
#4046=EDGE_CURVE('',#3195,#3194,#300,.T.);
#4047=EDGE_CURVE('',#3195,#3196,#301,.T.);
#4048=EDGE_CURVE('',#3197,#3196,#302,.T.);
#4049=EDGE_CURVE('',#3197,#3128,#2013,.T.);
#4050=EDGE_CURVE('',#3185,#3198,#303,.T.);
#4051=EDGE_CURVE('',#3198,#3199,#304,.T.);
#4052=EDGE_CURVE('',#3131,#3199,#2014,.T.);
#4053=EDGE_CURVE('',#3181,#3200,#305,.T.);
#4054=EDGE_CURVE('',#3135,#3200,#2015,.T.);
#4055=EDGE_CURVE('',#3177,#3201,#306,.T.);
#4056=EDGE_CURVE('',#3139,#3201,#2016,.T.);
#4057=EDGE_CURVE('',#3202,#3203,#307,.T.);
#4058=EDGE_CURVE('',#3203,#3204,#308,.T.);
#4059=EDGE_CURVE('',#3204,#3205,#2017,.T.);
#4060=EDGE_CURVE('',#3205,#3206,#309,.T.);
#4061=EDGE_CURVE('',#3206,#3207,#310,.T.);
#4062=EDGE_CURVE('',#3202,#3207,#2018,.T.);
#4063=EDGE_CURVE('',#3208,#3208,#2741,.T.);
#4064=EDGE_CURVE('',#3208,#3155,#2019,.T.);
#4065=EDGE_CURVE('',#3091,#3154,#2020,.T.);
#4066=EDGE_CURVE('',#3202,#3209,#311,.T.);
#4067=EDGE_CURVE('',#3210,#3207,#312,.T.);
#4068=EDGE_CURVE('',#3211,#3210,#313,.T.);
#4069=EDGE_CURVE('',#3212,#3211,#2021,.T.);
#4070=EDGE_CURVE('',#3209,#3212,#314,.T.);
#4071=EDGE_CURVE('',#3170,#3162,#315,.T.);
#4072=EDGE_CURVE('',#3209,#3213,#316,.T.);
#4073=EDGE_CURVE('',#3213,#3203,#317,.T.);
#4074=EDGE_CURVE('',#3163,#3169,#318,.T.);
#4075=EDGE_CURVE('',#3214,#3212,#319,.T.);
#4076=EDGE_CURVE('',#3213,#3214,#2742,.F.);
#4077=EDGE_CURVE('',#3168,#3164,#320,.T.);
#4078=EDGE_CURVE('',#3211,#3215,#321,.T.);
#4079=EDGE_CURVE('',#3215,#3214,#2022,.T.);
#4080=EDGE_CURVE('',#3165,#3167,#322,.T.);
#4081=EDGE_CURVE('',#3206,#3216,#323,.T.);
#4082=EDGE_CURVE('',#3216,#3210,#324,.T.);
#4083=EDGE_CURVE('',#3217,#3201,#325,.T.);
#4084=EDGE_CURVE('',#3218,#3217,#326,.T.);
#4085=EDGE_CURVE('',#3219,#3218,#2023,.T.);
#4086=EDGE_CURVE('',#3220,#3219,#327,.T.);
#4087=EDGE_CURVE('',#3186,#3220,#328,.T.);
#4088=EDGE_CURVE('',#3176,#3217,#329,.T.);
#4089=EDGE_CURVE('',#3218,#3175,#330,.T.);
#4090=EDGE_CURVE('',#3174,#3219,#331,.T.);
#4091=EDGE_CURVE('',#3220,#3173,#332,.T.);
#4092=EDGE_CURVE('',#3221,#3200,#333,.T.);
#4093=EDGE_CURVE('',#3083,#3221,#334,.T.);
#4094=EDGE_CURVE('',#3222,#3082,#335,.T.);
#4095=EDGE_CURVE('',#3187,#3222,#336,.T.);
#4096=EDGE_CURVE('',#3180,#3221,#337,.T.);
#4097=EDGE_CURVE('',#3222,#3179,#338,.T.);
#4098=EDGE_CURVE('',#3223,#3199,#339,.T.);
#4099=EDGE_CURVE('',#3224,#3223,#340,.T.);
#4100=EDGE_CURVE('',#3225,#3224,#2024,.T.);
#4101=EDGE_CURVE('',#3226,#3225,#341,.T.);
#4102=EDGE_CURVE('',#3188,#3226,#342,.T.);
#4103=EDGE_CURVE('',#3198,#3227,#343,.T.);
#4104=EDGE_CURVE('',#3227,#3223,#344,.T.);
#4105=EDGE_CURVE('',#3228,#3227,#2743,.F.);
#4106=EDGE_CURVE('',#3224,#3228,#345,.T.);
#4107=EDGE_CURVE('',#3228,#3229,#2025,.T.);
#4108=EDGE_CURVE('',#3229,#3225,#346,.T.);
#4109=EDGE_CURVE('',#3226,#3230,#347,.T.);
#4110=EDGE_CURVE('',#3230,#3189,#348,.T.);
#4111=EDGE_CURVE('',#3230,#3229,#2744,.F.);
#4112=EDGE_CURVE('',#3229,#3183,#2745,.F.);
#4113=EDGE_CURVE('',#3183,#3230,#2746,.F.);
#4114=EDGE_CURVE('',#3215,#3216,#2747,.F.);
#4115=EDGE_CURVE('',#3216,#3231,#2748,.F.);
#4116=EDGE_CURVE('',#3231,#3215,#2749,.F.);
#4117=EDGE_CURVE('',#3227,#3184,#2750,.F.);
#4118=EDGE_CURVE('',#3184,#3228,#2751,.F.);
#4119=EDGE_CURVE('',#3232,#3213,#2752,.F.);
#4120=EDGE_CURVE('',#3214,#3232,#2753,.F.);
#4121=EDGE_CURVE('',#3232,#3231,#2026,.T.);
#4122=EDGE_CURVE('',#3204,#3232,#349,.T.);
#4123=EDGE_CURVE('',#3231,#3205,#350,.T.);
#4124=EDGE_CURVE('',#3233,#3234,#2754,.F.);
#4125=EDGE_CURVE('',#3235,#3233,#2755,.F.);
#4126=EDGE_CURVE('',#3234,#3235,#2756,.F.);
#4127=EDGE_CURVE('',#3236,#3237,#2757,.F.);
#4128=EDGE_CURVE('',#3238,#3236,#2758,.F.);
#4129=EDGE_CURVE('',#3237,#3238,#2759,.F.);
#4130=EDGE_CURVE('',#3239,#3240,#2760,.F.);
#4131=EDGE_CURVE('',#3241,#3239,#2761,.F.);
#4132=EDGE_CURVE('',#3240,#3241,#2762,.F.);
#4133=EDGE_CURVE('',#3234,#3241,#2027,.T.);
#4134=EDGE_CURVE('',#3239,#3233,#2028,.T.);
#4135=EDGE_CURVE('',#3196,#3240,#351,.T.);
#4136=EDGE_CURVE('',#3241,#3197,#352,.T.);
#4137=EDGE_CURVE('',#3242,#3243,#2763,.F.);
#4138=EDGE_CURVE('',#3244,#3242,#2764,.F.);
#4139=EDGE_CURVE('',#3243,#3244,#2765,.F.);
#4140=EDGE_CURVE('',#3242,#3238,#2029,.T.);
#4141=EDGE_CURVE('',#3236,#3244,#2030,.T.);
#4142=EDGE_CURVE('',#3240,#3243,#353,.T.);
#4143=EDGE_CURVE('',#3244,#3239,#354,.T.);
#4144=EDGE_CURVE('',#3194,#3242,#355,.T.);
#4145=EDGE_CURVE('',#3243,#3195,#356,.T.);
#4146=EDGE_CURVE('',#3192,#3237,#357,.T.);
#4147=EDGE_CURVE('',#3238,#3193,#358,.T.);
#4148=EDGE_CURVE('',#3237,#3235,#359,.T.);
#4149=EDGE_CURVE('',#3233,#3236,#360,.T.);
#4150=EDGE_CURVE('',#3190,#3234,#361,.T.);
#4151=EDGE_CURVE('',#3235,#3191,#362,.T.);
#4152=EDGE_CURVE('',#3245,#3245,#2766,.T.);
#4153=EDGE_CURVE('',#3245,#3246,#2031,.T.);
#4154=EDGE_CURVE('',#3246,#3246,#2767,.T.);
#4155=EDGE_CURVE('',#3247,#3247,#2768,.T.);
#4156=EDGE_CURVE('',#3247,#3248,#2032,.T.);
#4157=EDGE_CURVE('',#3248,#3248,#2769,.T.);
#4158=EDGE_CURVE('',#3249,#3249,#2770,.T.);
#4159=EDGE_CURVE('',#3250,#3250,#2771,.T.);
#4160=EDGE_CURVE('',#3251,#3251,#2772,.T.);
#4161=EDGE_CURVE('',#3251,#3249,#2033,.T.);
#4162=EDGE_CURVE('',#3252,#3252,#2773,.T.);
#4163=EDGE_CURVE('',#3253,#3253,#2774,.T.);
#4164=EDGE_CURVE('',#3254,#3254,#2775,.T.);
#4165=EDGE_CURVE('',#3254,#3252,#2034,.T.);
#4166=EDGE_CURVE('',#3255,#3255,#2776,.T.);
#4167=EDGE_CURVE('',#3256,#3256,#2777,.T.);
#4168=EDGE_CURVE('',#3257,#3257,#2778,.T.);
#4169=EDGE_CURVE('',#3257,#3255,#2035,.T.);
#4170=EDGE_CURVE('',#3258,#3258,#2779,.T.);
#4171=EDGE_CURVE('',#3259,#3259,#2780,.T.);
#4172=EDGE_CURVE('',#3260,#3260,#2781,.T.);
#4173=EDGE_CURVE('',#3260,#3258,#2036,.T.);
#4174=EDGE_CURVE('',#3250,#3261,#2037,.T.);
#4175=EDGE_CURVE('',#3261,#3261,#2782,.T.);
#4176=EDGE_CURVE('',#3253,#3262,#2038,.T.);
#4177=EDGE_CURVE('',#3262,#3262,#2783,.T.);
#4178=EDGE_CURVE('',#3256,#3263,#2039,.T.);
#4179=EDGE_CURVE('',#3263,#3263,#2784,.T.);
#4180=EDGE_CURVE('',#3259,#3264,#2040,.T.);
#4181=EDGE_CURVE('',#3264,#3264,#2785,.T.);
#4182=EDGE_CURVE('',#3265,#3266,#2786,.T.);
#4183=EDGE_CURVE('',#3266,#3267,#363,.T.);
#4184=EDGE_CURVE('',#3267,#3268,#2787,.T.);
#4185=EDGE_CURVE('',#3268,#3265,#364,.T.);
#4186=EDGE_CURVE('',#3269,#3270,#2788,.T.);
#4187=EDGE_CURVE('',#3270,#3266,#2041,.T.);
#4188=EDGE_CURVE('',#3265,#3269,#2042,.T.);
#4189=EDGE_CURVE('',#3271,#3272,#2789,.T.);
#4190=EDGE_CURVE('',#3272,#3270,#365,.T.);
#4191=EDGE_CURVE('',#3269,#3271,#366,.T.);
#4192=EDGE_CURVE('',#3273,#3274,#2790,.T.);
#4193=EDGE_CURVE('',#3274,#3272,#367,.T.);
#4194=EDGE_CURVE('',#3271,#3273,#368,.T.);
#4195=EDGE_CURVE('',#3275,#3276,#2791,.T.);
#4196=EDGE_CURVE('',#3276,#3274,#369,.T.);
#4197=EDGE_CURVE('',#3273,#3275,#370,.T.);
#4198=EDGE_CURVE('',#3277,#3278,#2792,.T.);
#4199=EDGE_CURVE('',#3278,#3276,#2043,.T.);
#4200=EDGE_CURVE('',#3275,#3277,#2044,.T.);
#4201=EDGE_CURVE('',#3279,#3280,#2793,.T.);
#4202=EDGE_CURVE('',#3280,#3278,#371,.T.);
#4203=EDGE_CURVE('',#3277,#3279,#372,.T.);
#4204=EDGE_CURVE('',#3267,#3280,#373,.T.);
#4205=EDGE_CURVE('',#3279,#3268,#374,.T.);
#4206=EDGE_CURVE('',#3281,#3278,#375,.T.);
#4207=EDGE_CURVE('',#3282,#3281,#2045,.T.);
#4208=EDGE_CURVE('',#3276,#3282,#376,.T.);
#4209=EDGE_CURVE('',#3280,#3283,#377,.T.);
#4210=EDGE_CURVE('',#3283,#3281,#378,.T.);
#4211=EDGE_CURVE('',#3284,#3267,#379,.T.);
#4212=EDGE_CURVE('',#3283,#3284,#380,.T.);
#4213=EDGE_CURVE('',#3266,#3285,#381,.T.);
#4214=EDGE_CURVE('',#3285,#3284,#382,.T.);
#4215=EDGE_CURVE('',#3286,#3270,#383,.T.);
#4216=EDGE_CURVE('',#3285,#3286,#2046,.T.);
#4217=EDGE_CURVE('',#3282,#3287,#384,.T.);
#4218=EDGE_CURVE('',#3287,#3274,#385,.T.);
#4219=EDGE_CURVE('',#3272,#3288,#386,.T.);
#4220=EDGE_CURVE('',#3288,#3286,#387,.T.);
#4221=EDGE_CURVE('',#3288,#3287,#388,.T.);
#4222=EDGE_CURVE('',#3289,#3290,#2047,.T.);
#4223=EDGE_CURVE('',#3289,#3291,#389,.T.);
#4224=EDGE_CURVE('',#3291,#3292,#2794,.F.);
#4225=EDGE_CURVE('',#3292,#3290,#390,.T.);
#4226=EDGE_CURVE('',#3293,#3294,#2048,.T.);
#4227=EDGE_CURVE('',#3293,#3289,#391,.T.);
#4228=EDGE_CURVE('',#3290,#3294,#392,.T.);
#4229=EDGE_CURVE('',#3295,#3296,#2049,.T.);
#4230=EDGE_CURVE('',#3295,#3293,#393,.T.);
#4231=EDGE_CURVE('',#3294,#3296,#394,.T.);
#4232=EDGE_CURVE('',#3297,#3298,#2050,.T.);
#4233=EDGE_CURVE('',#3297,#3295,#395,.T.);
#4234=EDGE_CURVE('',#3296,#3298,#396,.T.);
#4235=EDGE_CURVE('',#3299,#3300,#2051,.T.);
#4236=EDGE_CURVE('',#3299,#3297,#397,.T.);
#4237=EDGE_CURVE('',#3298,#3300,#398,.T.);
#4238=EDGE_CURVE('',#3301,#3302,#2052,.T.);
#4239=EDGE_CURVE('',#3301,#3299,#399,.T.);
#4240=EDGE_CURVE('',#3300,#3302,#400,.T.);
#4241=EDGE_CURVE('',#3303,#3304,#2053,.T.);
#4242=EDGE_CURVE('',#3303,#3301,#401,.T.);
#4243=EDGE_CURVE('',#3302,#3304,#402,.T.);
#4244=EDGE_CURVE('',#3305,#3306,#2054,.T.);
#4245=EDGE_CURVE('',#3305,#3303,#403,.T.);
#4246=EDGE_CURVE('',#3304,#3306,#404,.T.);
#4247=EDGE_CURVE('',#3307,#3308,#2055,.T.);
#4248=EDGE_CURVE('',#3307,#3305,#405,.T.);
#4249=EDGE_CURVE('',#3306,#3308,#406,.T.);
#4250=EDGE_CURVE('',#3309,#3310,#2056,.T.);
#4251=EDGE_CURVE('',#3309,#3307,#407,.T.);
#4252=EDGE_CURVE('',#3308,#3310,#408,.T.);
#4253=EDGE_CURVE('',#3311,#3312,#2057,.T.);
#4254=EDGE_CURVE('',#3311,#3309,#409,.T.);
#4255=EDGE_CURVE('',#3310,#3312,#410,.T.);
#4256=EDGE_CURVE('',#3313,#3314,#2058,.T.);
#4257=EDGE_CURVE('',#3313,#3311,#411,.T.);
#4258=EDGE_CURVE('',#3312,#3314,#412,.T.);
#4259=EDGE_CURVE('',#3315,#3316,#2059,.T.);
#4260=EDGE_CURVE('',#3315,#3313,#413,.T.);
#4261=EDGE_CURVE('',#3314,#3316,#414,.T.);
#4262=EDGE_CURVE('',#3317,#3318,#2060,.T.);
#4263=EDGE_CURVE('',#3317,#3315,#415,.T.);
#4264=EDGE_CURVE('',#3316,#3318,#416,.T.);
#4265=EDGE_CURVE('',#3319,#3320,#2061,.T.);
#4266=EDGE_CURVE('',#3319,#3317,#417,.T.);
#4267=EDGE_CURVE('',#3318,#3320,#418,.T.);
#4268=EDGE_CURVE('',#3321,#3322,#2062,.T.);
#4269=EDGE_CURVE('',#3321,#3319,#419,.T.);
#4270=EDGE_CURVE('',#3320,#3322,#420,.T.);
#4271=EDGE_CURVE('',#3323,#3324,#2063,.T.);
#4272=EDGE_CURVE('',#3323,#3321,#421,.T.);
#4273=EDGE_CURVE('',#3322,#3324,#422,.T.);
#4274=EDGE_CURVE('',#3325,#3326,#2064,.T.);
#4275=EDGE_CURVE('',#3325,#3323,#423,.T.);
#4276=EDGE_CURVE('',#3324,#3326,#424,.T.);
#4277=EDGE_CURVE('',#3327,#3328,#2065,.T.);
#4278=EDGE_CURVE('',#3327,#3325,#425,.T.);
#4279=EDGE_CURVE('',#3326,#3328,#426,.T.);
#4280=EDGE_CURVE('',#3329,#3330,#2066,.T.);
#4281=EDGE_CURVE('',#3329,#3327,#427,.T.);
#4282=EDGE_CURVE('',#3328,#3330,#428,.T.);
#4283=EDGE_CURVE('',#3331,#3332,#2067,.T.);
#4284=EDGE_CURVE('',#3331,#3329,#429,.T.);
#4285=EDGE_CURVE('',#3330,#3332,#430,.T.);
#4286=EDGE_CURVE('',#3333,#3334,#2068,.T.);
#4287=EDGE_CURVE('',#3333,#3331,#431,.T.);
#4288=EDGE_CURVE('',#3332,#3334,#432,.T.);
#4289=EDGE_CURVE('',#3335,#3336,#2069,.T.);
#4290=EDGE_CURVE('',#3335,#3333,#433,.T.);
#4291=EDGE_CURVE('',#3334,#3336,#434,.T.);
#4292=EDGE_CURVE('',#3337,#3338,#2070,.T.);
#4293=EDGE_CURVE('',#3337,#3335,#435,.T.);
#4294=EDGE_CURVE('',#3336,#3338,#436,.T.);
#4295=EDGE_CURVE('',#3339,#3340,#2071,.T.);
#4296=EDGE_CURVE('',#3339,#3337,#437,.T.);
#4297=EDGE_CURVE('',#3338,#3340,#438,.T.);
#4298=EDGE_CURVE('',#3341,#3342,#2072,.T.);
#4299=EDGE_CURVE('',#3341,#3339,#439,.T.);
#4300=EDGE_CURVE('',#3340,#3342,#440,.T.);
#4301=EDGE_CURVE('',#3343,#3344,#2073,.T.);
#4302=EDGE_CURVE('',#3343,#3341,#441,.T.);
#4303=EDGE_CURVE('',#3342,#3344,#442,.T.);
#4304=EDGE_CURVE('',#3345,#3346,#2074,.T.);
#4305=EDGE_CURVE('',#3345,#3343,#443,.T.);
#4306=EDGE_CURVE('',#3344,#3346,#444,.T.);
#4307=EDGE_CURVE('',#3347,#3348,#2075,.T.);
#4308=EDGE_CURVE('',#3347,#3345,#445,.T.);
#4309=EDGE_CURVE('',#3346,#3348,#446,.T.);
#4310=EDGE_CURVE('',#3349,#3350,#2076,.T.);
#4311=EDGE_CURVE('',#3349,#3347,#447,.T.);
#4312=EDGE_CURVE('',#3348,#3350,#448,.T.);
#4313=EDGE_CURVE('',#3351,#3352,#2077,.T.);
#4314=EDGE_CURVE('',#3351,#3353,#449,.T.);
#4315=EDGE_CURVE('',#3353,#3354,#2795,.T.);
#4316=EDGE_CURVE('',#3352,#3354,#450,.T.);
#4317=EDGE_CURVE('',#3355,#3356,#2078,.T.);
#4318=EDGE_CURVE('',#3355,#3351,#451,.T.);
#4319=EDGE_CURVE('',#3356,#3352,#452,.T.);
#4320=EDGE_CURVE('',#3357,#3358,#2079,.T.);
#4321=EDGE_CURVE('',#3357,#3355,#453,.T.);
#4322=EDGE_CURVE('',#3358,#3356,#454,.T.);
#4323=EDGE_CURVE('',#3359,#3360,#2080,.T.);
#4324=EDGE_CURVE('',#3359,#3357,#455,.T.);
#4325=EDGE_CURVE('',#3360,#3358,#456,.T.);
#4326=EDGE_CURVE('',#3361,#3362,#2081,.T.);
#4327=EDGE_CURVE('',#3361,#3359,#457,.T.);
#4328=EDGE_CURVE('',#3362,#3360,#458,.T.);
#4329=EDGE_CURVE('',#3363,#3364,#2082,.T.);
#4330=EDGE_CURVE('',#3363,#3361,#459,.T.);
#4331=EDGE_CURVE('',#3364,#3362,#460,.T.);
#4332=EDGE_CURVE('',#3365,#3366,#2083,.T.);
#4333=EDGE_CURVE('',#3365,#3363,#461,.T.);
#4334=EDGE_CURVE('',#3366,#3364,#462,.T.);
#4335=EDGE_CURVE('',#3367,#3368,#2084,.T.);
#4336=EDGE_CURVE('',#3367,#3365,#463,.T.);
#4337=EDGE_CURVE('',#3368,#3366,#464,.T.);
#4338=EDGE_CURVE('',#3369,#3370,#2085,.T.);
#4339=EDGE_CURVE('',#3369,#3367,#465,.T.);
#4340=EDGE_CURVE('',#3370,#3368,#466,.T.);
#4341=EDGE_CURVE('',#3371,#3372,#2086,.T.);
#4342=EDGE_CURVE('',#3371,#3369,#467,.T.);
#4343=EDGE_CURVE('',#3372,#3370,#468,.T.);
#4344=EDGE_CURVE('',#3373,#3374,#2087,.T.);
#4345=EDGE_CURVE('',#3373,#3371,#469,.T.);
#4346=EDGE_CURVE('',#3374,#3372,#470,.T.);
#4347=EDGE_CURVE('',#3375,#3376,#2088,.T.);
#4348=EDGE_CURVE('',#3375,#3373,#471,.T.);
#4349=EDGE_CURVE('',#3376,#3374,#472,.T.);
#4350=EDGE_CURVE('',#3377,#3378,#2089,.T.);
#4351=EDGE_CURVE('',#3377,#3375,#473,.T.);
#4352=EDGE_CURVE('',#3378,#3376,#474,.T.);
#4353=EDGE_CURVE('',#3379,#3380,#2090,.T.);
#4354=EDGE_CURVE('',#3379,#3377,#475,.T.);
#4355=EDGE_CURVE('',#3380,#3378,#476,.T.);
#4356=EDGE_CURVE('',#3381,#3382,#2091,.T.);
#4357=EDGE_CURVE('',#3381,#3379,#477,.T.);
#4358=EDGE_CURVE('',#3382,#3380,#478,.T.);
#4359=EDGE_CURVE('',#3383,#3384,#2092,.T.);
#4360=EDGE_CURVE('',#3383,#3381,#479,.T.);
#4361=EDGE_CURVE('',#3384,#3382,#480,.T.);
#4362=EDGE_CURVE('',#3385,#3386,#2093,.T.);
#4363=EDGE_CURVE('',#3385,#3383,#481,.T.);
#4364=EDGE_CURVE('',#3386,#3384,#482,.T.);
#4365=EDGE_CURVE('',#3387,#3388,#2094,.T.);
#4366=EDGE_CURVE('',#3387,#3385,#483,.T.);
#4367=EDGE_CURVE('',#3388,#3386,#484,.T.);
#4368=EDGE_CURVE('',#3389,#3390,#2095,.T.);
#4369=EDGE_CURVE('',#3389,#3387,#485,.T.);
#4370=EDGE_CURVE('',#3390,#3388,#486,.T.);
#4371=EDGE_CURVE('',#3391,#3392,#2096,.T.);
#4372=EDGE_CURVE('',#3391,#3389,#487,.T.);
#4373=EDGE_CURVE('',#3392,#3390,#488,.T.);
#4374=EDGE_CURVE('',#3393,#3394,#2097,.T.);
#4375=EDGE_CURVE('',#3393,#3391,#489,.T.);
#4376=EDGE_CURVE('',#3394,#3392,#490,.T.);
#4377=EDGE_CURVE('',#3395,#3396,#2098,.T.);
#4378=EDGE_CURVE('',#3395,#3393,#491,.T.);
#4379=EDGE_CURVE('',#3396,#3394,#492,.T.);
#4380=EDGE_CURVE('',#3397,#3398,#2099,.T.);
#4381=EDGE_CURVE('',#3397,#3395,#493,.T.);
#4382=EDGE_CURVE('',#3398,#3396,#494,.T.);
#4383=EDGE_CURVE('',#3399,#3400,#2100,.T.);
#4384=EDGE_CURVE('',#3399,#3397,#495,.T.);
#4385=EDGE_CURVE('',#3400,#3398,#496,.T.);
#4386=EDGE_CURVE('',#3401,#3402,#2101,.T.);
#4387=EDGE_CURVE('',#3401,#3399,#497,.T.);
#4388=EDGE_CURVE('',#3402,#3400,#498,.T.);
#4389=EDGE_CURVE('',#3403,#3404,#2102,.T.);
#4390=EDGE_CURVE('',#3403,#3401,#499,.T.);
#4391=EDGE_CURVE('',#3404,#3402,#500,.T.);
#4392=EDGE_CURVE('',#3405,#3406,#2103,.T.);
#4393=EDGE_CURVE('',#3405,#3403,#501,.T.);
#4394=EDGE_CURVE('',#3406,#3404,#502,.T.);
#4395=EDGE_CURVE('',#3407,#3408,#2104,.T.);
#4396=EDGE_CURVE('',#3407,#3405,#503,.T.);
#4397=EDGE_CURVE('',#3408,#3406,#504,.T.);
#4398=EDGE_CURVE('',#3409,#3410,#2105,.T.);
#4399=EDGE_CURVE('',#3409,#3407,#505,.T.);
#4400=EDGE_CURVE('',#3410,#3408,#506,.T.);
#4401=EDGE_CURVE('',#3411,#3412,#2106,.T.);
#4402=EDGE_CURVE('',#3411,#3409,#507,.T.);
#4403=EDGE_CURVE('',#3412,#3410,#508,.T.);
#4404=EDGE_CURVE('',#3354,#3413,#509,.T.);
#4405=EDGE_CURVE('',#3414,#3353,#510,.T.);
#4406=EDGE_CURVE('',#3415,#3414,#2796,.T.);
#4407=EDGE_CURVE('',#3413,#3415,#511,.T.);
#4408=EDGE_CURVE('',#3413,#3416,#2107,.T.);
#4409=EDGE_CURVE('',#3416,#3416,#2797,.T.);
#4410=EDGE_CURVE('',#3417,#3411,#512,.T.);
#4411=EDGE_CURVE('',#3291,#3417,#513,.T.);
#4412=EDGE_CURVE('',#3414,#3349,#514,.T.);
#4413=EDGE_CURVE('',#3418,#3412,#515,.T.);
#4414=EDGE_CURVE('',#3417,#3418,#2798,.T.);
#4415=EDGE_CURVE('',#3350,#3415,#516,.T.);
#4416=EDGE_CURVE('',#3418,#3292,#517,.T.);
#4417=EDGE_CURVE('',#3419,#3420,#2108,.T.);
#4418=EDGE_CURVE('',#3419,#3421,#2109,.T.);
#4419=EDGE_CURVE('',#3421,#3422,#2110,.T.);
#4420=EDGE_CURVE('',#3420,#3422,#2111,.T.);
#4421=EDGE_CURVE('',#3423,#3419,#2112,.T.);
#4422=EDGE_CURVE('',#3423,#3424,#2113,.T.);
#4423=EDGE_CURVE('',#3424,#3421,#2114,.T.);
#4424=EDGE_CURVE('',#3425,#3423,#2115,.T.);
#4425=EDGE_CURVE('',#3425,#3426,#2116,.T.);
#4426=EDGE_CURVE('',#3426,#3424,#2117,.T.);
#4427=EDGE_CURVE('',#3427,#3425,#2118,.T.);
#4428=EDGE_CURVE('',#3427,#3428,#2119,.T.);
#4429=EDGE_CURVE('',#3428,#3426,#2120,.T.);
#4430=EDGE_CURVE('',#3429,#3427,#2121,.T.);
#4431=EDGE_CURVE('',#3429,#3430,#2122,.T.);
#4432=EDGE_CURVE('',#3430,#3428,#2123,.T.);
#4433=EDGE_CURVE('',#3420,#3429,#2124,.T.);
#4434=EDGE_CURVE('',#3422,#3430,#2125,.T.);
#4435=EDGE_CURVE('',#3431,#3431,#2799,.T.);
#4436=EDGE_CURVE('',#3431,#3432,#2126,.T.);
#4437=EDGE_CURVE('',#3432,#3432,#2800,.T.);
#4438=EDGE_CURVE('',#3433,#3434,#2127,.T.);
#4439=EDGE_CURVE('',#3435,#3434,#2801,.F.);
#4440=EDGE_CURVE('',#3435,#3433,#518,.T.);
#4441=EDGE_CURVE('',#3436,#3437,#2128,.T.);
#4442=EDGE_CURVE('',#3437,#3438,#519,.T.);
#4443=EDGE_CURVE('',#3434,#3438,#2802,.F.);
#4444=EDGE_CURVE('',#3433,#3436,#520,.T.);
#4445=EDGE_CURVE('',#3439,#3440,#2129,.T.);
#4446=EDGE_CURVE('',#3440,#3437,#521,.T.);
#4447=EDGE_CURVE('',#3436,#3439,#522,.T.);
#4448=EDGE_CURVE('',#3441,#3442,#2130,.T.);
#4449=EDGE_CURVE('',#3442,#3440,#523,.T.);
#4450=EDGE_CURVE('',#3439,#3441,#524,.T.);
#4451=EDGE_CURVE('',#3443,#3444,#2131,.T.);
#4452=EDGE_CURVE('',#3443,#3445,#525,.T.);
#4453=EDGE_CURVE('',#3446,#3445,#2803,.T.);
#4454=EDGE_CURVE('',#3446,#3444,#526,.T.);
#4455=EDGE_CURVE('',#3447,#3448,#2132,.T.);
#4456=EDGE_CURVE('',#3448,#3449,#527,.T.);
#4457=EDGE_CURVE('',#3450,#3449,#2804,.T.);
#4458=EDGE_CURVE('',#3447,#3450,#528,.T.);
#4459=EDGE_CURVE('',#3451,#3452,#2133,.T.);
#4460=EDGE_CURVE('',#3452,#3448,#529,.T.);
#4461=EDGE_CURVE('',#3451,#3447,#530,.T.);
#4462=EDGE_CURVE('',#3453,#3454,#2134,.T.);
#4463=EDGE_CURVE('',#3454,#3452,#531,.T.);
#4464=EDGE_CURVE('',#3453,#3451,#532,.T.);
#4465=EDGE_CURVE('',#3455,#3456,#2135,.T.);
#4466=EDGE_CURVE('',#3456,#3454,#533,.T.);
#4467=EDGE_CURVE('',#3455,#3453,#534,.T.);
#4468=EDGE_CURVE('',#3457,#3458,#2136,.T.);
#4469=EDGE_CURVE('',#3459,#3457,#535,.T.);
#4470=EDGE_CURVE('',#3460,#3459,#2805,.T.);
#4471=EDGE_CURVE('',#3460,#3458,#536,.T.);
#4472=EDGE_CURVE('',#3458,#3456,#537,.T.);
#4473=EDGE_CURVE('',#3457,#3455,#538,.T.);
#4474=EDGE_CURVE('',#3449,#3435,#539,.T.);
#4475=EDGE_CURVE('',#3445,#3460,#540,.T.);
#4476=EDGE_CURVE('',#3441,#3443,#541,.T.);
#4477=EDGE_CURVE('',#3438,#3450,#542,.T.);
#4478=EDGE_CURVE('',#3444,#3442,#543,.T.);
#4479=EDGE_CURVE('',#3459,#3446,#544,.T.);
#4480=EDGE_CURVE('',#3461,#3462,#2137,.T.);
#4481=EDGE_CURVE('',#3462,#3463,#2138,.T.);
#4482=EDGE_CURVE('',#3463,#3464,#2139,.T.);
#4483=EDGE_CURVE('',#3464,#3465,#2140,.T.);
#4484=EDGE_CURVE('',#3465,#3466,#2141,.T.);
#4485=EDGE_CURVE('',#3466,#3461,#2142,.T.);
#4486=EDGE_CURVE('',#3467,#3468,#2143,.T.);
#4487=EDGE_CURVE('',#3468,#3461,#2144,.T.);
#4488=EDGE_CURVE('',#3467,#3466,#2145,.T.);
#4489=EDGE_CURVE('',#3469,#3467,#2146,.T.);
#4490=EDGE_CURVE('',#3469,#3465,#2147,.T.);
#4491=EDGE_CURVE('',#3470,#3469,#2148,.T.);
#4492=EDGE_CURVE('',#3470,#3464,#2149,.T.);
#4493=EDGE_CURVE('',#3471,#3470,#2150,.T.);
#4494=EDGE_CURVE('',#3471,#3463,#2151,.T.);
#4495=EDGE_CURVE('',#3472,#3471,#2152,.T.);
#4496=EDGE_CURVE('',#3472,#3462,#2153,.T.);
#4497=EDGE_CURVE('',#3468,#3472,#2154,.T.);
#4498=EDGE_CURVE('',#3473,#3473,#2806,.T.);
#4499=EDGE_CURVE('',#3473,#3474,#2155,.T.);
#4500=EDGE_CURVE('',#3474,#3474,#2807,.T.);
#4501=EDGE_CURVE('',#3475,#3475,#2808,.T.);
#4502=EDGE_CURVE('',#3475,#3476,#2156,.T.);
#4503=EDGE_CURVE('',#3476,#3476,#2809,.T.);
#4504=ORIENTED_EDGE('',*,*,#3477,.F.);
#4505=ORIENTED_EDGE('',*,*,#3478,.T.);
#4506=ORIENTED_EDGE('',*,*,#3479,.F.);
#4507=ORIENTED_EDGE('',*,*,#3478,.F.);
#4508=ORIENTED_EDGE('',*,*,#3480,.F.);
#4509=ORIENTED_EDGE('',*,*,#3481,.T.);
#4510=ORIENTED_EDGE('',*,*,#3482,.F.);
#4511=ORIENTED_EDGE('',*,*,#3481,.F.);
#4512=ORIENTED_EDGE('',*,*,#3483,.F.);
#4513=ORIENTED_EDGE('',*,*,#3484,.T.);
#4514=ORIENTED_EDGE('',*,*,#3485,.F.);
#4515=ORIENTED_EDGE('',*,*,#3484,.F.);
#4516=ORIENTED_EDGE('',*,*,#3486,.F.);
#4517=ORIENTED_EDGE('',*,*,#3487,.F.);
#4518=ORIENTED_EDGE('',*,*,#3488,.T.);
#4519=ORIENTED_EDGE('',*,*,#3489,.F.);
#4520=ORIENTED_EDGE('',*,*,#3490,.T.);
#4521=ORIENTED_EDGE('',*,*,#3487,.T.);
#4522=ORIENTED_EDGE('',*,*,#3491,.F.);
#4523=ORIENTED_EDGE('',*,*,#3492,.F.);
#4524=ORIENTED_EDGE('',*,*,#3493,.F.);
#4525=ORIENTED_EDGE('',*,*,#3489,.T.);
#4526=ORIENTED_EDGE('',*,*,#3494,.F.);
#4527=ORIENTED_EDGE('',*,*,#3495,.F.);
#4528=ORIENTED_EDGE('',*,*,#3488,.F.);
#4529=ORIENTED_EDGE('',*,*,#3496,.F.);
#4530=ORIENTED_EDGE('',*,*,#3497,.F.);
#4531=ORIENTED_EDGE('',*,*,#3498,.T.);
#4532=ORIENTED_EDGE('',*,*,#3499,.F.);
#4533=ORIENTED_EDGE('',*,*,#3500,.F.);
#4534=ORIENTED_EDGE('',*,*,#3501,.T.);
#4535=ORIENTED_EDGE('',*,*,#3493,.T.);
#4536=ORIENTED_EDGE('',*,*,#3502,.F.);
#4537=ORIENTED_EDGE('',*,*,#3503,.F.);
#4538=ORIENTED_EDGE('',*,*,#3504,.T.);
#4539=ORIENTED_EDGE('',*,*,#3503,.T.);
#4540=ORIENTED_EDGE('',*,*,#3505,.F.);
#4541=ORIENTED_EDGE('',*,*,#3498,.F.);
#4542=ORIENTED_EDGE('',*,*,#3486,.T.);
#4543=ORIENTED_EDGE('',*,*,#3495,.T.);
#4544=ORIENTED_EDGE('',*,*,#3506,.F.);
#4545=ORIENTED_EDGE('',*,*,#3507,.F.);
#4546=ORIENTED_EDGE('',*,*,#3499,.T.);
#4547=ORIENTED_EDGE('',*,*,#3505,.T.);
#4548=ORIENTED_EDGE('',*,*,#3502,.T.);
#4549=ORIENTED_EDGE('',*,*,#3492,.T.);
#4550=ORIENTED_EDGE('',*,*,#3491,.T.);
#4551=ORIENTED_EDGE('',*,*,#3500,.T.);
#4552=ORIENTED_EDGE('',*,*,#3507,.T.);
#4553=ORIENTED_EDGE('',*,*,#3508,.T.);
#4554=ORIENTED_EDGE('',*,*,#3509,.F.);
#4555=ORIENTED_EDGE('',*,*,#3510,.F.);
#4556=ORIENTED_EDGE('',*,*,#3511,.F.);
#4557=ORIENTED_EDGE('',*,*,#3506,.T.);
#4558=ORIENTED_EDGE('',*,*,#3494,.T.);
#4559=ORIENTED_EDGE('',*,*,#3512,.F.);
#4560=ORIENTED_EDGE('',*,*,#3513,.T.);
#4561=ORIENTED_EDGE('',*,*,#3514,.F.);
#4562=ORIENTED_EDGE('',*,*,#3508,.F.);
#4563=ORIENTED_EDGE('',*,*,#3515,.F.);
#4564=ORIENTED_EDGE('',*,*,#3516,.F.);
#4565=ORIENTED_EDGE('',*,*,#3513,.F.);
#4566=ORIENTED_EDGE('',*,*,#3517,.F.);
#4567=ORIENTED_EDGE('',*,*,#3518,.F.);
#4568=ORIENTED_EDGE('',*,*,#3519,.F.);
#4569=ORIENTED_EDGE('',*,*,#3510,.T.);
#4570=ORIENTED_EDGE('',*,*,#3520,.F.);
#4571=ORIENTED_EDGE('',*,*,#3515,.T.);
#4572=ORIENTED_EDGE('',*,*,#3521,.T.);
#4573=ORIENTED_EDGE('',*,*,#3522,.T.);
#4574=ORIENTED_EDGE('',*,*,#3523,.F.);
#4575=ORIENTED_EDGE('',*,*,#3518,.T.);
#4576=ORIENTED_EDGE('',*,*,#3524,.F.);
#4577=ORIENTED_EDGE('',*,*,#3525,.T.);
#4578=ORIENTED_EDGE('',*,*,#3526,.T.);
#4579=ORIENTED_EDGE('',*,*,#3523,.T.);
#4580=ORIENTED_EDGE('',*,*,#3527,.T.);
#4581=ORIENTED_EDGE('',*,*,#3528,.T.);
#4582=ORIENTED_EDGE('',*,*,#3529,.T.);
#4583=ORIENTED_EDGE('',*,*,#3530,.T.);
#4584=ORIENTED_EDGE('',*,*,#3531,.T.);
#4585=ORIENTED_EDGE('',*,*,#3532,.T.);
#4586=ORIENTED_EDGE('',*,*,#3533,.T.);
#4587=ORIENTED_EDGE('',*,*,#3534,.T.);
#4588=ORIENTED_EDGE('',*,*,#3535,.T.);
#4589=ORIENTED_EDGE('',*,*,#3536,.T.);
#4590=ORIENTED_EDGE('',*,*,#3524,.T.);
#4591=ORIENTED_EDGE('',*,*,#3520,.T.);
#4592=ORIENTED_EDGE('',*,*,#3509,.T.);
#4593=ORIENTED_EDGE('',*,*,#3514,.T.);
#4594=ORIENTED_EDGE('',*,*,#3516,.T.);
#4595=ORIENTED_EDGE('',*,*,#3477,.T.);
#4596=ORIENTED_EDGE('',*,*,#3480,.T.);
#4597=ORIENTED_EDGE('',*,*,#3483,.T.);
#4598=ORIENTED_EDGE('',*,*,#3537,.F.);
#4599=ORIENTED_EDGE('',*,*,#3538,.T.);
#4600=ORIENTED_EDGE('',*,*,#3539,.T.);
#4601=ORIENTED_EDGE('',*,*,#3540,.T.);
#4602=ORIENTED_EDGE('',*,*,#3539,.F.);
#4603=ORIENTED_EDGE('',*,*,#3541,.F.);
#4604=ORIENTED_EDGE('',*,*,#3542,.F.);
#4605=ORIENTED_EDGE('',*,*,#3543,.T.);
#4606=ORIENTED_EDGE('',*,*,#3540,.F.);
#4607=ORIENTED_EDGE('',*,*,#3543,.F.);
#4608=ORIENTED_EDGE('',*,*,#3511,.T.);
#4609=ORIENTED_EDGE('',*,*,#3519,.T.);
#4610=ORIENTED_EDGE('',*,*,#3526,.F.);
#4611=ORIENTED_EDGE('',*,*,#3544,.F.);
#4612=ORIENTED_EDGE('',*,*,#3545,.F.);
#4613=ORIENTED_EDGE('',*,*,#3546,.F.);
#4614=ORIENTED_EDGE('',*,*,#3547,.F.);
#4615=ORIENTED_EDGE('',*,*,#3548,.F.);
#4616=ORIENTED_EDGE('',*,*,#3549,.F.);
#4617=ORIENTED_EDGE('',*,*,#3550,.F.);
#4618=ORIENTED_EDGE('',*,*,#3551,.F.);
#4619=ORIENTED_EDGE('',*,*,#3552,.F.);
#4620=ORIENTED_EDGE('',*,*,#3553,.F.);
#4621=ORIENTED_EDGE('',*,*,#3521,.F.);
#4622=ORIENTED_EDGE('',*,*,#3517,.T.);
#4623=ORIENTED_EDGE('',*,*,#3512,.T.);
#4624=ORIENTED_EDGE('',*,*,#3496,.T.);
#4625=ORIENTED_EDGE('',*,*,#3490,.F.);
#4626=ORIENTED_EDGE('',*,*,#3501,.F.);
#4627=ORIENTED_EDGE('',*,*,#3504,.F.);
#4628=ORIENTED_EDGE('',*,*,#3497,.T.);
#4629=ORIENTED_EDGE('',*,*,#3479,.T.);
#4630=ORIENTED_EDGE('',*,*,#3482,.T.);
#4631=ORIENTED_EDGE('',*,*,#3485,.T.);
#4632=ORIENTED_EDGE('',*,*,#3538,.F.);
#4633=ORIENTED_EDGE('',*,*,#3537,.T.);
#4634=ORIENTED_EDGE('',*,*,#3554,.T.);
#4635=ORIENTED_EDGE('',*,*,#3541,.T.);
#4636=ORIENTED_EDGE('',*,*,#3542,.T.);
#4637=ORIENTED_EDGE('',*,*,#3554,.F.);
#4638=ORIENTED_EDGE('',*,*,#3555,.F.);
#4639=ORIENTED_EDGE('',*,*,#3534,.F.);
#4640=ORIENTED_EDGE('',*,*,#3556,.F.);
#4641=ORIENTED_EDGE('',*,*,#3546,.T.);
#4642=ORIENTED_EDGE('',*,*,#3557,.F.);
#4643=ORIENTED_EDGE('',*,*,#3552,.T.);
#4644=ORIENTED_EDGE('',*,*,#3558,.F.);
#4645=ORIENTED_EDGE('',*,*,#3528,.F.);
#4646=ORIENTED_EDGE('',*,*,#3558,.T.);
#4647=ORIENTED_EDGE('',*,*,#3551,.T.);
#4648=ORIENTED_EDGE('',*,*,#3559,.T.);
#4649=ORIENTED_EDGE('',*,*,#3529,.F.);
#4650=ORIENTED_EDGE('',*,*,#3556,.T.);
#4651=ORIENTED_EDGE('',*,*,#3533,.F.);
#4652=ORIENTED_EDGE('',*,*,#3560,.F.);
#4653=ORIENTED_EDGE('',*,*,#3547,.T.);
#4654=ORIENTED_EDGE('',*,*,#3557,.T.);
#4655=ORIENTED_EDGE('',*,*,#3527,.F.);
#4656=ORIENTED_EDGE('',*,*,#3522,.F.);
#4657=ORIENTED_EDGE('',*,*,#3553,.T.);
#4658=ORIENTED_EDGE('',*,*,#3525,.F.);
#4659=ORIENTED_EDGE('',*,*,#3536,.F.);
#4660=ORIENTED_EDGE('',*,*,#3561,.F.);
#4661=ORIENTED_EDGE('',*,*,#3544,.T.);
#4662=ORIENTED_EDGE('',*,*,#3555,.T.);
#4663=ORIENTED_EDGE('',*,*,#3545,.T.);
#4664=ORIENTED_EDGE('',*,*,#3561,.T.);
#4665=ORIENTED_EDGE('',*,*,#3535,.F.);
#4666=ORIENTED_EDGE('',*,*,#3548,.T.);
#4667=ORIENTED_EDGE('',*,*,#3560,.T.);
#4668=ORIENTED_EDGE('',*,*,#3532,.F.);
#4669=ORIENTED_EDGE('',*,*,#3562,.F.);
#4670=ORIENTED_EDGE('',*,*,#3549,.T.);
#4671=ORIENTED_EDGE('',*,*,#3562,.T.);
#4672=ORIENTED_EDGE('',*,*,#3531,.F.);
#4673=ORIENTED_EDGE('',*,*,#3563,.F.);
#4674=ORIENTED_EDGE('',*,*,#3550,.T.);
#4675=ORIENTED_EDGE('',*,*,#3563,.T.);
#4676=ORIENTED_EDGE('',*,*,#3530,.F.);
#4677=ORIENTED_EDGE('',*,*,#3559,.F.);
#4678=ORIENTED_EDGE('',*,*,#3564,.F.);
#4679=ORIENTED_EDGE('',*,*,#3565,.T.);
#4680=ORIENTED_EDGE('',*,*,#3566,.F.);
#4681=ORIENTED_EDGE('',*,*,#3565,.F.);
#4682=ORIENTED_EDGE('',*,*,#3567,.F.);
#4683=ORIENTED_EDGE('',*,*,#3568,.T.);
#4684=ORIENTED_EDGE('',*,*,#3569,.F.);
#4685=ORIENTED_EDGE('',*,*,#3568,.F.);
#4686=ORIENTED_EDGE('',*,*,#3570,.F.);
#4687=ORIENTED_EDGE('',*,*,#3571,.T.);
#4688=ORIENTED_EDGE('',*,*,#3572,.F.);
#4689=ORIENTED_EDGE('',*,*,#3571,.F.);
#4690=ORIENTED_EDGE('',*,*,#3573,.T.);
#4691=ORIENTED_EDGE('',*,*,#3574,.F.);
#4692=ORIENTED_EDGE('',*,*,#3575,.F.);
#4693=ORIENTED_EDGE('',*,*,#3576,.F.);
#4694=ORIENTED_EDGE('',*,*,#3577,.F.);
#4695=ORIENTED_EDGE('',*,*,#3578,.T.);
#4696=ORIENTED_EDGE('',*,*,#3579,.F.);
#4697=ORIENTED_EDGE('',*,*,#3580,.F.);
#4698=ORIENTED_EDGE('',*,*,#3581,.T.);
#4699=ORIENTED_EDGE('',*,*,#3575,.T.);
#4700=ORIENTED_EDGE('',*,*,#3582,.F.);
#4701=ORIENTED_EDGE('',*,*,#3583,.F.);
#4702=ORIENTED_EDGE('',*,*,#3584,.T.);
#4703=ORIENTED_EDGE('',*,*,#3583,.T.);
#4704=ORIENTED_EDGE('',*,*,#3585,.F.);
#4705=ORIENTED_EDGE('',*,*,#3586,.F.);
#4706=ORIENTED_EDGE('',*,*,#3587,.T.);
#4707=ORIENTED_EDGE('',*,*,#3586,.T.);
#4708=ORIENTED_EDGE('',*,*,#3588,.F.);
#4709=ORIENTED_EDGE('',*,*,#3578,.F.);
#4710=ORIENTED_EDGE('',*,*,#3589,.F.);
#4711=ORIENTED_EDGE('',*,*,#3579,.T.);
#4712=ORIENTED_EDGE('',*,*,#3588,.T.);
#4713=ORIENTED_EDGE('',*,*,#3585,.T.);
#4714=ORIENTED_EDGE('',*,*,#3582,.T.);
#4715=ORIENTED_EDGE('',*,*,#3574,.T.);
#4716=ORIENTED_EDGE('',*,*,#3590,.F.);
#4717=ORIENTED_EDGE('',*,*,#3580,.T.);
#4718=ORIENTED_EDGE('',*,*,#3589,.T.);
#4719=ORIENTED_EDGE('',*,*,#3591,.T.);
#4720=ORIENTED_EDGE('',*,*,#3592,.F.);
#4721=ORIENTED_EDGE('',*,*,#3593,.F.);
#4722=ORIENTED_EDGE('',*,*,#3594,.F.);
#4723=ORIENTED_EDGE('',*,*,#3590,.T.);
#4724=ORIENTED_EDGE('',*,*,#3595,.T.);
#4725=ORIENTED_EDGE('',*,*,#3596,.F.);
#4726=ORIENTED_EDGE('',*,*,#3591,.F.);
#4727=ORIENTED_EDGE('',*,*,#3597,.F.);
#4728=ORIENTED_EDGE('',*,*,#3598,.F.);
#4729=ORIENTED_EDGE('',*,*,#3595,.F.);
#4730=ORIENTED_EDGE('',*,*,#3573,.F.);
#4731=ORIENTED_EDGE('',*,*,#3599,.F.);
#4732=ORIENTED_EDGE('',*,*,#3600,.F.);
#4733=ORIENTED_EDGE('',*,*,#3601,.F.);
#4734=ORIENTED_EDGE('',*,*,#3593,.T.);
#4735=ORIENTED_EDGE('',*,*,#3602,.F.);
#4736=ORIENTED_EDGE('',*,*,#3597,.T.);
#4737=ORIENTED_EDGE('',*,*,#3603,.T.);
#4738=ORIENTED_EDGE('',*,*,#3604,.T.);
#4739=ORIENTED_EDGE('',*,*,#3605,.F.);
#4740=ORIENTED_EDGE('',*,*,#3600,.T.);
#4741=ORIENTED_EDGE('',*,*,#3606,.F.);
#4742=ORIENTED_EDGE('',*,*,#3607,.T.);
#4743=ORIENTED_EDGE('',*,*,#3608,.T.);
#4744=ORIENTED_EDGE('',*,*,#3605,.T.);
#4745=ORIENTED_EDGE('',*,*,#3609,.T.);
#4746=ORIENTED_EDGE('',*,*,#3610,.T.);
#4747=ORIENTED_EDGE('',*,*,#3611,.T.);
#4748=ORIENTED_EDGE('',*,*,#3612,.T.);
#4749=ORIENTED_EDGE('',*,*,#3613,.T.);
#4750=ORIENTED_EDGE('',*,*,#3614,.T.);
#4751=ORIENTED_EDGE('',*,*,#3615,.T.);
#4752=ORIENTED_EDGE('',*,*,#3616,.T.);
#4753=ORIENTED_EDGE('',*,*,#3617,.T.);
#4754=ORIENTED_EDGE('',*,*,#3618,.T.);
#4755=ORIENTED_EDGE('',*,*,#3606,.T.);
#4756=ORIENTED_EDGE('',*,*,#3602,.T.);
#4757=ORIENTED_EDGE('',*,*,#3592,.T.);
#4758=ORIENTED_EDGE('',*,*,#3596,.T.);
#4759=ORIENTED_EDGE('',*,*,#3598,.T.);
#4760=ORIENTED_EDGE('',*,*,#3564,.T.);
#4761=ORIENTED_EDGE('',*,*,#3567,.T.);
#4762=ORIENTED_EDGE('',*,*,#3570,.T.);
#4763=ORIENTED_EDGE('',*,*,#3619,.F.);
#4764=ORIENTED_EDGE('',*,*,#3620,.T.);
#4765=ORIENTED_EDGE('',*,*,#3621,.T.);
#4766=ORIENTED_EDGE('',*,*,#3622,.T.);
#4767=ORIENTED_EDGE('',*,*,#3621,.F.);
#4768=ORIENTED_EDGE('',*,*,#3623,.F.);
#4769=ORIENTED_EDGE('',*,*,#3624,.F.);
#4770=ORIENTED_EDGE('',*,*,#3625,.T.);
#4771=ORIENTED_EDGE('',*,*,#3622,.F.);
#4772=ORIENTED_EDGE('',*,*,#3625,.F.);
#4773=ORIENTED_EDGE('',*,*,#3594,.T.);
#4774=ORIENTED_EDGE('',*,*,#3601,.T.);
#4775=ORIENTED_EDGE('',*,*,#3608,.F.);
#4776=ORIENTED_EDGE('',*,*,#3626,.F.);
#4777=ORIENTED_EDGE('',*,*,#3627,.F.);
#4778=ORIENTED_EDGE('',*,*,#3628,.F.);
#4779=ORIENTED_EDGE('',*,*,#3629,.F.);
#4780=ORIENTED_EDGE('',*,*,#3630,.F.);
#4781=ORIENTED_EDGE('',*,*,#3631,.F.);
#4782=ORIENTED_EDGE('',*,*,#3632,.F.);
#4783=ORIENTED_EDGE('',*,*,#3633,.F.);
#4784=ORIENTED_EDGE('',*,*,#3634,.F.);
#4785=ORIENTED_EDGE('',*,*,#3635,.F.);
#4786=ORIENTED_EDGE('',*,*,#3603,.F.);
#4787=ORIENTED_EDGE('',*,*,#3599,.T.);
#4788=ORIENTED_EDGE('',*,*,#3576,.T.);
#4789=ORIENTED_EDGE('',*,*,#3581,.F.);
#4790=ORIENTED_EDGE('',*,*,#3584,.F.);
#4791=ORIENTED_EDGE('',*,*,#3587,.F.);
#4792=ORIENTED_EDGE('',*,*,#3577,.T.);
#4793=ORIENTED_EDGE('',*,*,#3566,.T.);
#4794=ORIENTED_EDGE('',*,*,#3569,.T.);
#4795=ORIENTED_EDGE('',*,*,#3572,.T.);
#4796=ORIENTED_EDGE('',*,*,#3620,.F.);
#4797=ORIENTED_EDGE('',*,*,#3619,.T.);
#4798=ORIENTED_EDGE('',*,*,#3636,.T.);
#4799=ORIENTED_EDGE('',*,*,#3623,.T.);
#4800=ORIENTED_EDGE('',*,*,#3624,.T.);
#4801=ORIENTED_EDGE('',*,*,#3636,.F.);
#4802=ORIENTED_EDGE('',*,*,#3637,.F.);
#4803=ORIENTED_EDGE('',*,*,#3616,.F.);
#4804=ORIENTED_EDGE('',*,*,#3638,.F.);
#4805=ORIENTED_EDGE('',*,*,#3628,.T.);
#4806=ORIENTED_EDGE('',*,*,#3639,.F.);
#4807=ORIENTED_EDGE('',*,*,#3634,.T.);
#4808=ORIENTED_EDGE('',*,*,#3640,.F.);
#4809=ORIENTED_EDGE('',*,*,#3610,.F.);
#4810=ORIENTED_EDGE('',*,*,#3640,.T.);
#4811=ORIENTED_EDGE('',*,*,#3633,.T.);
#4812=ORIENTED_EDGE('',*,*,#3641,.T.);
#4813=ORIENTED_EDGE('',*,*,#3611,.F.);
#4814=ORIENTED_EDGE('',*,*,#3638,.T.);
#4815=ORIENTED_EDGE('',*,*,#3615,.F.);
#4816=ORIENTED_EDGE('',*,*,#3642,.F.);
#4817=ORIENTED_EDGE('',*,*,#3629,.T.);
#4818=ORIENTED_EDGE('',*,*,#3639,.T.);
#4819=ORIENTED_EDGE('',*,*,#3609,.F.);
#4820=ORIENTED_EDGE('',*,*,#3604,.F.);
#4821=ORIENTED_EDGE('',*,*,#3635,.T.);
#4822=ORIENTED_EDGE('',*,*,#3607,.F.);
#4823=ORIENTED_EDGE('',*,*,#3618,.F.);
#4824=ORIENTED_EDGE('',*,*,#3643,.F.);
#4825=ORIENTED_EDGE('',*,*,#3626,.T.);
#4826=ORIENTED_EDGE('',*,*,#3637,.T.);
#4827=ORIENTED_EDGE('',*,*,#3627,.T.);
#4828=ORIENTED_EDGE('',*,*,#3643,.T.);
#4829=ORIENTED_EDGE('',*,*,#3617,.F.);
#4830=ORIENTED_EDGE('',*,*,#3630,.T.);
#4831=ORIENTED_EDGE('',*,*,#3642,.T.);
#4832=ORIENTED_EDGE('',*,*,#3614,.F.);
#4833=ORIENTED_EDGE('',*,*,#3644,.F.);
#4834=ORIENTED_EDGE('',*,*,#3631,.T.);
#4835=ORIENTED_EDGE('',*,*,#3644,.T.);
#4836=ORIENTED_EDGE('',*,*,#3613,.F.);
#4837=ORIENTED_EDGE('',*,*,#3645,.F.);
#4838=ORIENTED_EDGE('',*,*,#3632,.T.);
#4839=ORIENTED_EDGE('',*,*,#3645,.T.);
#4840=ORIENTED_EDGE('',*,*,#3612,.F.);
#4841=ORIENTED_EDGE('',*,*,#3641,.F.);
#4842=ORIENTED_EDGE('',*,*,#3646,.T.);
#4843=ORIENTED_EDGE('',*,*,#3647,.T.);
#4844=ORIENTED_EDGE('',*,*,#3648,.F.);
#4845=ORIENTED_EDGE('',*,*,#3647,.F.);
#4846=ORIENTED_EDGE('',*,*,#3649,.F.);
#4847=ORIENTED_EDGE('',*,*,#3646,.F.);
#4848=ORIENTED_EDGE('',*,*,#3650,.F.);
#4849=ORIENTED_EDGE('',*,*,#3648,.T.);
#4850=ORIENTED_EDGE('',*,*,#3651,.F.);
#4851=ORIENTED_EDGE('',*,*,#3652,.T.);
#4852=ORIENTED_EDGE('',*,*,#3650,.T.);
#4853=ORIENTED_EDGE('',*,*,#3652,.F.);
#4854=ORIENTED_EDGE('',*,*,#3653,.T.);
#4855=ORIENTED_EDGE('',*,*,#3654,.F.);
#4856=ORIENTED_EDGE('',*,*,#3653,.F.);
#4857=ORIENTED_EDGE('',*,*,#3655,.T.);
#4858=ORIENTED_EDGE('',*,*,#3656,.T.);
#4859=ORIENTED_EDGE('',*,*,#3655,.F.);
#4860=ORIENTED_EDGE('',*,*,#3656,.F.);
#4861=ORIENTED_EDGE('',*,*,#3649,.T.);
#4862=ORIENTED_EDGE('',*,*,#3657,.T.);
#4863=ORIENTED_EDGE('',*,*,#3654,.T.);
#4864=ORIENTED_EDGE('',*,*,#3657,.F.);
#4865=ORIENTED_EDGE('',*,*,#3651,.T.);
#4866=ORIENTED_EDGE('',*,*,#3658,.F.);
#4867=ORIENTED_EDGE('',*,*,#3659,.F.);
#4868=ORIENTED_EDGE('',*,*,#3660,.F.);
#4869=ORIENTED_EDGE('',*,*,#3661,.F.);
#4870=ORIENTED_EDGE('',*,*,#3662,.F.);
#4871=ORIENTED_EDGE('',*,*,#3663,.F.);
#4872=ORIENTED_EDGE('',*,*,#3664,.F.);
#4873=ORIENTED_EDGE('',*,*,#3665,.F.);
#4874=ORIENTED_EDGE('',*,*,#3665,.T.);
#4875=ORIENTED_EDGE('',*,*,#3666,.F.);
#4876=ORIENTED_EDGE('',*,*,#3659,.T.);
#4877=ORIENTED_EDGE('',*,*,#3667,.F.);
#4878=ORIENTED_EDGE('',*,*,#3662,.T.);
#4879=ORIENTED_EDGE('',*,*,#3667,.T.);
#4880=ORIENTED_EDGE('',*,*,#3658,.T.);
#4881=ORIENTED_EDGE('',*,*,#3668,.F.);
#4882=ORIENTED_EDGE('',*,*,#3664,.T.);
#4883=ORIENTED_EDGE('',*,*,#3669,.F.);
#4884=ORIENTED_EDGE('',*,*,#3660,.T.);
#4885=ORIENTED_EDGE('',*,*,#3666,.T.);
#4886=ORIENTED_EDGE('',*,*,#3663,.T.);
#4887=ORIENTED_EDGE('',*,*,#3668,.T.);
#4888=ORIENTED_EDGE('',*,*,#3661,.T.);
#4889=ORIENTED_EDGE('',*,*,#3669,.T.);
#4890=ORIENTED_EDGE('',*,*,#3670,.T.);
#4891=ORIENTED_EDGE('',*,*,#3671,.T.);
#4892=ORIENTED_EDGE('',*,*,#3672,.T.);
#4893=ORIENTED_EDGE('',*,*,#3673,.F.);
#4894=ORIENTED_EDGE('',*,*,#3674,.T.);
#4895=ORIENTED_EDGE('',*,*,#3675,.T.);
#4896=ORIENTED_EDGE('',*,*,#3676,.T.);
#4897=ORIENTED_EDGE('',*,*,#3677,.F.);
#4898=ORIENTED_EDGE('',*,*,#3678,.T.);
#4899=ORIENTED_EDGE('',*,*,#3679,.T.);
#4900=ORIENTED_EDGE('',*,*,#3680,.T.);
#4901=ORIENTED_EDGE('',*,*,#3681,.F.);
#4902=ORIENTED_EDGE('',*,*,#3682,.T.);
#4903=ORIENTED_EDGE('',*,*,#3683,.F.);
#4904=ORIENTED_EDGE('',*,*,#3682,.F.);
#4905=ORIENTED_EDGE('',*,*,#3684,.F.);
#4906=ORIENTED_EDGE('',*,*,#3685,.T.);
#4907=ORIENTED_EDGE('',*,*,#3679,.F.);
#4908=ORIENTED_EDGE('',*,*,#3685,.F.);
#4909=ORIENTED_EDGE('',*,*,#3686,.F.);
#4910=ORIENTED_EDGE('',*,*,#3687,.T.);
#4911=ORIENTED_EDGE('',*,*,#3678,.F.);
#4912=ORIENTED_EDGE('',*,*,#3687,.F.);
#4913=ORIENTED_EDGE('',*,*,#3688,.F.);
#4914=ORIENTED_EDGE('',*,*,#3689,.T.);
#4915=ORIENTED_EDGE('',*,*,#3690,.F.);
#4916=ORIENTED_EDGE('',*,*,#3689,.F.);
#4917=ORIENTED_EDGE('',*,*,#3691,.F.);
#4918=ORIENTED_EDGE('',*,*,#3692,.T.);
#4919=ORIENTED_EDGE('',*,*,#3693,.T.);
#4920=ORIENTED_EDGE('',*,*,#3692,.F.);
#4921=ORIENTED_EDGE('',*,*,#3693,.F.);
#4922=ORIENTED_EDGE('',*,*,#3694,.F.);
#4923=ORIENTED_EDGE('',*,*,#3695,.F.);
#4924=ORIENTED_EDGE('',*,*,#3696,.T.);
#4925=ORIENTED_EDGE('',*,*,#3697,.T.);
#4926=ORIENTED_EDGE('',*,*,#3696,.F.);
#4927=ORIENTED_EDGE('',*,*,#3697,.F.);
#4928=ORIENTED_EDGE('',*,*,#3698,.F.);
#4929=ORIENTED_EDGE('',*,*,#3694,.T.);
#4930=ORIENTED_EDGE('',*,*,#3699,.T.);
#4931=ORIENTED_EDGE('',*,*,#3700,.F.);
#4932=ORIENTED_EDGE('',*,*,#3699,.F.);
#4933=ORIENTED_EDGE('',*,*,#3698,.T.);
#4934=ORIENTED_EDGE('',*,*,#3701,.T.);
#4935=ORIENTED_EDGE('',*,*,#3702,.F.);
#4936=ORIENTED_EDGE('',*,*,#3701,.F.);
#4937=ORIENTED_EDGE('',*,*,#3703,.F.);
#4938=ORIENTED_EDGE('',*,*,#3704,.F.);
#4939=ORIENTED_EDGE('',*,*,#3705,.F.);
#4940=ORIENTED_EDGE('',*,*,#3706,.T.);
#4941=ORIENTED_EDGE('',*,*,#3707,.F.);
#4942=ORIENTED_EDGE('',*,*,#3708,.T.);
#4943=ORIENTED_EDGE('',*,*,#3709,.F.);
#4944=ORIENTED_EDGE('',*,*,#3710,.F.);
#4945=ORIENTED_EDGE('',*,*,#3711,.F.);
#4946=ORIENTED_EDGE('',*,*,#3712,.T.);
#4947=ORIENTED_EDGE('',*,*,#3713,.F.);
#4948=ORIENTED_EDGE('',*,*,#3714,.F.);
#4949=ORIENTED_EDGE('',*,*,#3715,.F.);
#4950=ORIENTED_EDGE('',*,*,#3716,.T.);
#4951=ORIENTED_EDGE('',*,*,#3717,.F.);
#4952=ORIENTED_EDGE('',*,*,#3718,.F.);
#4953=ORIENTED_EDGE('',*,*,#3719,.F.);
#4954=ORIENTED_EDGE('',*,*,#3720,.T.);
#4955=ORIENTED_EDGE('',*,*,#3721,.F.);
#4956=ORIENTED_EDGE('',*,*,#3722,.F.);
#4957=ORIENTED_EDGE('',*,*,#3723,.F.);
#4958=ORIENTED_EDGE('',*,*,#3724,.F.);
#4959=ORIENTED_EDGE('',*,*,#3725,.F.);
#4960=ORIENTED_EDGE('',*,*,#3726,.T.);
#4961=ORIENTED_EDGE('',*,*,#3727,.F.);
#4962=ORIENTED_EDGE('',*,*,#3728,.F.);
#4963=ORIENTED_EDGE('',*,*,#3729,.F.);
#4964=ORIENTED_EDGE('',*,*,#3730,.T.);
#4965=ORIENTED_EDGE('',*,*,#3731,.F.);
#4966=ORIENTED_EDGE('',*,*,#3700,.T.);
#4967=ORIENTED_EDGE('',*,*,#3732,.F.);
#4968=ORIENTED_EDGE('',*,*,#3702,.T.);
#4969=ORIENTED_EDGE('',*,*,#3733,.F.);
#4970=ORIENTED_EDGE('',*,*,#3706,.F.);
#4971=ORIENTED_EDGE('',*,*,#3734,.F.);
#4972=ORIENTED_EDGE('',*,*,#3720,.F.);
#4973=ORIENTED_EDGE('',*,*,#3735,.F.);
#4974=ORIENTED_EDGE('',*,*,#3726,.F.);
#4975=ORIENTED_EDGE('',*,*,#3736,.F.);
#4976=ORIENTED_EDGE('',*,*,#3708,.F.);
#4977=ORIENTED_EDGE('',*,*,#3737,.F.);
#4978=ORIENTED_EDGE('',*,*,#3730,.F.);
#4979=ORIENTED_EDGE('',*,*,#3738,.F.);
#4980=ORIENTED_EDGE('',*,*,#3712,.F.);
#4981=ORIENTED_EDGE('',*,*,#3739,.F.);
#4982=ORIENTED_EDGE('',*,*,#3740,.F.);
#4983=ORIENTED_EDGE('',*,*,#3741,.F.);
#4984=ORIENTED_EDGE('',*,*,#3716,.F.);
#4985=ORIENTED_EDGE('',*,*,#3742,.F.);
#4986=ORIENTED_EDGE('',*,*,#3743,.F.);
#4987=ORIENTED_EDGE('',*,*,#3744,.F.);
#4988=ORIENTED_EDGE('',*,*,#3740,.T.);
#4989=ORIENTED_EDGE('',*,*,#3745,.T.);
#4990=ORIENTED_EDGE('',*,*,#3746,.F.);
#4991=ORIENTED_EDGE('',*,*,#3747,.F.);
#4992=ORIENTED_EDGE('',*,*,#3748,.F.);
#4993=ORIENTED_EDGE('',*,*,#3749,.F.);
#4994=ORIENTED_EDGE('',*,*,#3750,.F.);
#4995=ORIENTED_EDGE('',*,*,#3717,.T.);
#4996=ORIENTED_EDGE('',*,*,#3741,.T.);
#4997=ORIENTED_EDGE('',*,*,#3744,.T.);
#4998=ORIENTED_EDGE('',*,*,#3751,.T.);
#4999=ORIENTED_EDGE('',*,*,#3752,.F.);
#5000=ORIENTED_EDGE('',*,*,#3753,.F.);
#5001=ORIENTED_EDGE('',*,*,#3754,.F.);
#5002=ORIENTED_EDGE('',*,*,#3755,.F.);
#5003=ORIENTED_EDGE('',*,*,#3756,.F.);
#5004=ORIENTED_EDGE('',*,*,#3757,.T.);
#5005=ORIENTED_EDGE('',*,*,#3713,.T.);
#5006=ORIENTED_EDGE('',*,*,#3738,.T.);
#5007=ORIENTED_EDGE('',*,*,#3729,.T.);
#5008=ORIENTED_EDGE('',*,*,#3758,.T.);
#5009=ORIENTED_EDGE('',*,*,#3759,.F.);
#5010=ORIENTED_EDGE('',*,*,#3760,.F.);
#5011=ORIENTED_EDGE('',*,*,#3761,.F.);
#5012=ORIENTED_EDGE('',*,*,#3762,.F.);
#5013=ORIENTED_EDGE('',*,*,#3763,.F.);
#5014=ORIENTED_EDGE('',*,*,#3764,.T.);
#5015=ORIENTED_EDGE('',*,*,#3709,.T.);
#5016=ORIENTED_EDGE('',*,*,#3736,.T.);
#5017=ORIENTED_EDGE('',*,*,#3725,.T.);
#5018=ORIENTED_EDGE('',*,*,#3765,.T.);
#5019=ORIENTED_EDGE('',*,*,#3766,.F.);
#5020=ORIENTED_EDGE('',*,*,#3767,.F.);
#5021=ORIENTED_EDGE('',*,*,#3675,.F.);
#5022=ORIENTED_EDGE('',*,*,#3768,.F.);
#5023=ORIENTED_EDGE('',*,*,#3769,.F.);
#5024=ORIENTED_EDGE('',*,*,#3770,.T.);
#5025=ORIENTED_EDGE('',*,*,#3703,.T.);
#5026=ORIENTED_EDGE('',*,*,#3733,.T.);
#5027=ORIENTED_EDGE('',*,*,#3719,.T.);
#5028=ORIENTED_EDGE('',*,*,#3771,.F.);
#5029=ORIENTED_EDGE('',*,*,#3772,.T.);
#5030=ORIENTED_EDGE('',*,*,#3773,.T.);
#5031=ORIENTED_EDGE('',*,*,#3774,.T.);
#5032=ORIENTED_EDGE('',*,*,#3775,.F.);
#5033=ORIENTED_EDGE('',*,*,#3718,.T.);
#5034=ORIENTED_EDGE('',*,*,#3757,.F.);
#5035=ORIENTED_EDGE('',*,*,#3776,.T.);
#5036=ORIENTED_EDGE('',*,*,#3745,.F.);
#5037=ORIENTED_EDGE('',*,*,#3777,.T.);
#5038=ORIENTED_EDGE('',*,*,#3751,.F.);
#5039=ORIENTED_EDGE('',*,*,#3743,.T.);
#5040=ORIENTED_EDGE('',*,*,#3778,.F.);
#5041=ORIENTED_EDGE('',*,*,#3779,.T.);
#5042=ORIENTED_EDGE('',*,*,#3758,.F.);
#5043=ORIENTED_EDGE('',*,*,#3728,.T.);
#5044=ORIENTED_EDGE('',*,*,#3780,.F.);
#5045=ORIENTED_EDGE('',*,*,#3781,.T.);
#5046=ORIENTED_EDGE('',*,*,#3765,.F.);
#5047=ORIENTED_EDGE('',*,*,#3724,.T.);
#5048=ORIENTED_EDGE('',*,*,#3782,.F.);
#5049=ORIENTED_EDGE('',*,*,#3783,.T.);
#5050=ORIENTED_EDGE('',*,*,#3784,.T.);
#5051=ORIENTED_EDGE('',*,*,#3771,.T.);
#5052=ORIENTED_EDGE('',*,*,#3722,.T.);
#5053=ORIENTED_EDGE('',*,*,#3785,.T.);
#5054=ORIENTED_EDGE('',*,*,#3786,.F.);
#5055=ORIENTED_EDGE('',*,*,#3787,.T.);
#5056=ORIENTED_EDGE('',*,*,#3788,.F.);
#5057=ORIENTED_EDGE('',*,*,#3789,.T.);
#5058=ORIENTED_EDGE('',*,*,#3790,.F.);
#5059=ORIENTED_EDGE('',*,*,#3791,.T.);
#5060=ORIENTED_EDGE('',*,*,#3792,.F.);
#5061=ORIENTED_EDGE('',*,*,#3793,.T.);
#5062=ORIENTED_EDGE('',*,*,#3704,.T.);
#5063=ORIENTED_EDGE('',*,*,#3775,.T.);
#5064=ORIENTED_EDGE('',*,*,#3794,.T.);
#5065=ORIENTED_EDGE('',*,*,#3795,.T.);
#5066=ORIENTED_EDGE('',*,*,#3796,.F.);
#5067=ORIENTED_EDGE('',*,*,#3710,.T.);
#5068=ORIENTED_EDGE('',*,*,#3770,.F.);
#5069=ORIENTED_EDGE('',*,*,#3797,.T.);
#5070=ORIENTED_EDGE('',*,*,#3798,.F.);
#5071=ORIENTED_EDGE('',*,*,#3714,.T.);
#5072=ORIENTED_EDGE('',*,*,#3764,.F.);
#5073=ORIENTED_EDGE('',*,*,#3799,.T.);
#5074=ORIENTED_EDGE('',*,*,#3800,.F.);
#5075=ORIENTED_EDGE('',*,*,#3801,.T.);
#5076=ORIENTED_EDGE('',*,*,#3802,.T.);
#5077=ORIENTED_EDGE('',*,*,#3803,.T.);
#5078=ORIENTED_EDGE('',*,*,#3804,.T.);
#5079=ORIENTED_EDGE('',*,*,#3805,.T.);
#5080=ORIENTED_EDGE('',*,*,#3806,.F.);
#5081=ORIENTED_EDGE('',*,*,#3807,.F.);
#5082=ORIENTED_EDGE('',*,*,#3808,.T.);
#5083=ORIENTED_EDGE('',*,*,#3732,.T.);
#5084=ORIENTED_EDGE('',*,*,#3808,.F.);
#5085=ORIENTED_EDGE('',*,*,#3680,.F.);
#5086=ORIENTED_EDGE('',*,*,#3809,.T.);
#5087=ORIENTED_EDGE('',*,*,#3731,.T.);
#5088=ORIENTED_EDGE('',*,*,#3809,.F.);
#5089=ORIENTED_EDGE('',*,*,#3810,.F.);
#5090=ORIENTED_EDGE('',*,*,#3806,.T.);
#5091=ORIENTED_EDGE('',*,*,#3811,.F.);
#5092=ORIENTED_EDGE('',*,*,#3812,.F.);
#5093=ORIENTED_EDGE('',*,*,#3813,.F.);
#5094=ORIENTED_EDGE('',*,*,#3814,.F.);
#5095=ORIENTED_EDGE('',*,*,#3746,.T.);
#5096=ORIENTED_EDGE('',*,*,#3776,.F.);
#5097=ORIENTED_EDGE('',*,*,#3756,.T.);
#5098=ORIENTED_EDGE('',*,*,#3815,.T.);
#5099=ORIENTED_EDGE('',*,*,#3810,.T.);
#5100=ORIENTED_EDGE('',*,*,#3816,.T.);
#5101=ORIENTED_EDGE('',*,*,#3817,.T.);
#5102=ORIENTED_EDGE('',*,*,#3801,.F.);
#5103=ORIENTED_EDGE('',*,*,#3747,.T.);
#5104=ORIENTED_EDGE('',*,*,#3815,.F.);
#5105=ORIENTED_EDGE('',*,*,#3755,.T.);
#5106=ORIENTED_EDGE('',*,*,#3818,.F.);
#5107=ORIENTED_EDGE('',*,*,#3814,.T.);
#5108=ORIENTED_EDGE('',*,*,#3819,.F.);
#5109=ORIENTED_EDGE('',*,*,#3820,.F.);
#5110=ORIENTED_EDGE('',*,*,#3816,.F.);
#5111=ORIENTED_EDGE('',*,*,#3748,.T.);
#5112=ORIENTED_EDGE('',*,*,#3818,.T.);
#5113=ORIENTED_EDGE('',*,*,#3754,.T.);
#5114=ORIENTED_EDGE('',*,*,#3821,.T.);
#5115=ORIENTED_EDGE('',*,*,#3683,.T.);
#5116=ORIENTED_EDGE('',*,*,#3690,.T.);
#5117=ORIENTED_EDGE('',*,*,#3807,.T.);
#5118=ORIENTED_EDGE('',*,*,#3813,.T.);
#5119=ORIENTED_EDGE('',*,*,#3822,.T.);
#5120=ORIENTED_EDGE('',*,*,#3823,.T.);
#5121=ORIENTED_EDGE('',*,*,#3819,.T.);
#5122=ORIENTED_EDGE('',*,*,#3749,.T.);
#5123=ORIENTED_EDGE('',*,*,#3821,.F.);
#5124=ORIENTED_EDGE('',*,*,#3753,.T.);
#5125=ORIENTED_EDGE('',*,*,#3824,.F.);
#5126=ORIENTED_EDGE('',*,*,#3750,.T.);
#5127=ORIENTED_EDGE('',*,*,#3824,.T.);
#5128=ORIENTED_EDGE('',*,*,#3752,.T.);
#5129=ORIENTED_EDGE('',*,*,#3777,.F.);
#5130=ORIENTED_EDGE('',*,*,#3811,.T.);
#5131=ORIENTED_EDGE('',*,*,#3805,.F.);
#5132=ORIENTED_EDGE('',*,*,#3825,.T.);
#5133=ORIENTED_EDGE('',*,*,#3826,.T.);
#5134=ORIENTED_EDGE('',*,*,#3715,.T.);
#5135=ORIENTED_EDGE('',*,*,#3800,.T.);
#5136=ORIENTED_EDGE('',*,*,#3827,.F.);
#5137=ORIENTED_EDGE('',*,*,#3828,.F.);
#5138=ORIENTED_EDGE('',*,*,#3829,.F.);
#5139=ORIENTED_EDGE('',*,*,#3830,.F.);
#5140=ORIENTED_EDGE('',*,*,#3831,.F.);
#5141=ORIENTED_EDGE('',*,*,#3778,.T.);
#5142=ORIENTED_EDGE('',*,*,#3742,.T.);
#5143=ORIENTED_EDGE('',*,*,#3739,.T.);
#5144=ORIENTED_EDGE('',*,*,#3827,.T.);
#5145=ORIENTED_EDGE('',*,*,#3799,.F.);
#5146=ORIENTED_EDGE('',*,*,#3763,.T.);
#5147=ORIENTED_EDGE('',*,*,#3832,.T.);
#5148=ORIENTED_EDGE('',*,*,#3828,.T.);
#5149=ORIENTED_EDGE('',*,*,#3832,.F.);
#5150=ORIENTED_EDGE('',*,*,#3762,.T.);
#5151=ORIENTED_EDGE('',*,*,#3833,.F.);
#5152=ORIENTED_EDGE('',*,*,#3829,.T.);
#5153=ORIENTED_EDGE('',*,*,#3833,.T.);
#5154=ORIENTED_EDGE('',*,*,#3761,.T.);
#5155=ORIENTED_EDGE('',*,*,#3834,.T.);
#5156=ORIENTED_EDGE('',*,*,#3830,.T.);
#5157=ORIENTED_EDGE('',*,*,#3834,.F.);
#5158=ORIENTED_EDGE('',*,*,#3760,.T.);
#5159=ORIENTED_EDGE('',*,*,#3835,.F.);
#5160=ORIENTED_EDGE('',*,*,#3831,.T.);
#5161=ORIENTED_EDGE('',*,*,#3835,.T.);
#5162=ORIENTED_EDGE('',*,*,#3759,.T.);
#5163=ORIENTED_EDGE('',*,*,#3779,.F.);
#5164=ORIENTED_EDGE('',*,*,#3711,.T.);
#5165=ORIENTED_EDGE('',*,*,#3798,.T.);
#5166=ORIENTED_EDGE('',*,*,#3836,.F.);
#5167=ORIENTED_EDGE('',*,*,#3837,.F.);
#5168=ORIENTED_EDGE('',*,*,#3671,.F.);
#5169=ORIENTED_EDGE('',*,*,#3838,.F.);
#5170=ORIENTED_EDGE('',*,*,#3839,.F.);
#5171=ORIENTED_EDGE('',*,*,#3780,.T.);
#5172=ORIENTED_EDGE('',*,*,#3727,.T.);
#5173=ORIENTED_EDGE('',*,*,#3737,.T.);
#5174=ORIENTED_EDGE('',*,*,#3836,.T.);
#5175=ORIENTED_EDGE('',*,*,#3797,.F.);
#5176=ORIENTED_EDGE('',*,*,#3769,.T.);
#5177=ORIENTED_EDGE('',*,*,#3840,.T.);
#5178=ORIENTED_EDGE('',*,*,#3673,.T.);
#5179=ORIENTED_EDGE('',*,*,#3672,.F.);
#5180=ORIENTED_EDGE('',*,*,#3837,.T.);
#5181=ORIENTED_EDGE('',*,*,#3840,.F.);
#5182=ORIENTED_EDGE('',*,*,#3768,.T.);
#5183=ORIENTED_EDGE('',*,*,#3674,.F.);
#5184=ORIENTED_EDGE('',*,*,#3677,.T.);
#5185=ORIENTED_EDGE('',*,*,#3676,.F.);
#5186=ORIENTED_EDGE('',*,*,#3767,.T.);
#5187=ORIENTED_EDGE('',*,*,#3841,.F.);
#5188=ORIENTED_EDGE('',*,*,#3838,.T.);
#5189=ORIENTED_EDGE('',*,*,#3670,.F.);
#5190=ORIENTED_EDGE('',*,*,#3839,.T.);
#5191=ORIENTED_EDGE('',*,*,#3841,.T.);
#5192=ORIENTED_EDGE('',*,*,#3766,.T.);
#5193=ORIENTED_EDGE('',*,*,#3781,.F.);
#5194=ORIENTED_EDGE('',*,*,#3707,.T.);
#5195=ORIENTED_EDGE('',*,*,#3796,.T.);
#5196=ORIENTED_EDGE('',*,*,#3842,.F.);
#5197=ORIENTED_EDGE('',*,*,#3843,.F.);
#5198=ORIENTED_EDGE('',*,*,#3844,.F.);
#5199=ORIENTED_EDGE('',*,*,#3845,.F.);
#5200=ORIENTED_EDGE('',*,*,#3846,.F.);
#5201=ORIENTED_EDGE('',*,*,#3782,.T.);
#5202=ORIENTED_EDGE('',*,*,#3723,.T.);
#5203=ORIENTED_EDGE('',*,*,#3735,.T.);
#5204=ORIENTED_EDGE('',*,*,#3842,.T.);
#5205=ORIENTED_EDGE('',*,*,#3795,.F.);
#5206=ORIENTED_EDGE('',*,*,#3847,.T.);
#5207=ORIENTED_EDGE('',*,*,#3848,.T.);
#5208=ORIENTED_EDGE('',*,*,#3843,.T.);
#5209=ORIENTED_EDGE('',*,*,#3848,.F.);
#5210=ORIENTED_EDGE('',*,*,#3849,.F.);
#5211=ORIENTED_EDGE('',*,*,#3850,.F.);
#5212=ORIENTED_EDGE('',*,*,#3844,.T.);
#5213=ORIENTED_EDGE('',*,*,#3850,.T.);
#5214=ORIENTED_EDGE('',*,*,#3851,.T.);
#5215=ORIENTED_EDGE('',*,*,#3852,.T.);
#5216=ORIENTED_EDGE('',*,*,#3846,.T.);
#5217=ORIENTED_EDGE('',*,*,#3853,.T.);
#5218=ORIENTED_EDGE('',*,*,#3854,.T.);
#5219=ORIENTED_EDGE('',*,*,#3783,.F.);
#5220=ORIENTED_EDGE('',*,*,#3845,.T.);
#5221=ORIENTED_EDGE('',*,*,#3852,.F.);
#5222=ORIENTED_EDGE('',*,*,#3855,.F.);
#5223=ORIENTED_EDGE('',*,*,#3853,.F.);
#5224=ORIENTED_EDGE('',*,*,#3856,.T.);
#5225=ORIENTED_EDGE('',*,*,#3857,.T.);
#5226=ORIENTED_EDGE('',*,*,#3855,.T.);
#5227=ORIENTED_EDGE('',*,*,#3858,.T.);
#5228=ORIENTED_EDGE('',*,*,#3859,.T.);
#5229=ORIENTED_EDGE('',*,*,#3860,.T.);
#5230=ORIENTED_EDGE('',*,*,#3849,.T.);
#5231=ORIENTED_EDGE('',*,*,#3861,.T.);
#5232=ORIENTED_EDGE('',*,*,#3862,.T.);
#5233=ORIENTED_EDGE('',*,*,#3856,.F.);
#5234=ORIENTED_EDGE('',*,*,#3851,.F.);
#5235=ORIENTED_EDGE('',*,*,#3862,.F.);
#5236=ORIENTED_EDGE('',*,*,#3773,.F.);
#5237=ORIENTED_EDGE('',*,*,#3794,.F.);
#5238=ORIENTED_EDGE('',*,*,#3774,.F.);
#5239=ORIENTED_EDGE('',*,*,#3861,.F.);
#5240=ORIENTED_EDGE('',*,*,#3847,.F.);
#5241=ORIENTED_EDGE('',*,*,#3863,.T.);
#5242=ORIENTED_EDGE('',*,*,#3820,.T.);
#5243=ORIENTED_EDGE('',*,*,#3864,.T.);
#5244=ORIENTED_EDGE('',*,*,#3864,.F.);
#5245=ORIENTED_EDGE('',*,*,#3823,.F.);
#5246=ORIENTED_EDGE('',*,*,#3860,.F.);
#5247=ORIENTED_EDGE('',*,*,#3865,.F.);
#5248=ORIENTED_EDGE('',*,*,#3802,.F.);
#5249=ORIENTED_EDGE('',*,*,#3817,.F.);
#5250=ORIENTED_EDGE('',*,*,#3863,.F.);
#5251=ORIENTED_EDGE('',*,*,#3866,.F.);
#5252=ORIENTED_EDGE('',*,*,#3804,.F.);
#5253=ORIENTED_EDGE('',*,*,#3867,.F.);
#5254=ORIENTED_EDGE('',*,*,#3859,.F.);
#5255=ORIENTED_EDGE('',*,*,#3825,.F.);
#5256=ORIENTED_EDGE('',*,*,#3812,.T.);
#5257=ORIENTED_EDGE('',*,*,#3826,.F.);
#5258=ORIENTED_EDGE('',*,*,#3858,.F.);
#5259=ORIENTED_EDGE('',*,*,#3822,.F.);
#5260=ORIENTED_EDGE('',*,*,#3784,.F.);
#5261=ORIENTED_EDGE('',*,*,#3854,.F.);
#5262=ORIENTED_EDGE('',*,*,#3857,.F.);
#5263=ORIENTED_EDGE('',*,*,#3772,.F.);
#5264=ORIENTED_EDGE('',*,*,#3866,.T.);
#5265=ORIENTED_EDGE('',*,*,#3865,.T.);
#5266=ORIENTED_EDGE('',*,*,#3867,.T.);
#5267=ORIENTED_EDGE('',*,*,#3803,.F.);
#5268=ORIENTED_EDGE('',*,*,#3868,.F.);
#5269=ORIENTED_EDGE('',*,*,#3869,.F.);
#5270=ORIENTED_EDGE('',*,*,#3870,.F.);
#5271=ORIENTED_EDGE('',*,*,#3871,.F.);
#5272=ORIENTED_EDGE('',*,*,#3872,.F.);
#5273=ORIENTED_EDGE('',*,*,#3873,.F.);
#5274=ORIENTED_EDGE('',*,*,#3874,.F.);
#5275=ORIENTED_EDGE('',*,*,#3875,.F.);
#5276=ORIENTED_EDGE('',*,*,#3876,.F.);
#5277=ORIENTED_EDGE('',*,*,#3868,.T.);
#5278=ORIENTED_EDGE('',*,*,#3877,.T.);
#5279=ORIENTED_EDGE('',*,*,#3875,.T.);
#5280=ORIENTED_EDGE('',*,*,#3878,.T.);
#5281=ORIENTED_EDGE('',*,*,#3792,.T.);
#5282=ORIENTED_EDGE('',*,*,#3879,.T.);
#5283=ORIENTED_EDGE('',*,*,#3876,.T.);
#5284=ORIENTED_EDGE('',*,*,#3880,.T.);
#5285=ORIENTED_EDGE('',*,*,#3881,.F.);
#5286=ORIENTED_EDGE('',*,*,#3882,.F.);
#5287=ORIENTED_EDGE('',*,*,#3883,.F.);
#5288=ORIENTED_EDGE('',*,*,#3882,.T.);
#5289=ORIENTED_EDGE('',*,*,#3884,.T.);
#5290=ORIENTED_EDGE('',*,*,#3872,.T.);
#5291=ORIENTED_EDGE('',*,*,#3885,.T.);
#5292=ORIENTED_EDGE('',*,*,#3874,.T.);
#5293=ORIENTED_EDGE('',*,*,#3886,.T.);
#5294=ORIENTED_EDGE('',*,*,#3883,.T.);
#5295=ORIENTED_EDGE('',*,*,#3887,.T.);
#5296=ORIENTED_EDGE('',*,*,#3790,.T.);
#5297=ORIENTED_EDGE('',*,*,#3888,.T.);
#5298=ORIENTED_EDGE('',*,*,#3881,.T.);
#5299=ORIENTED_EDGE('',*,*,#3889,.T.);
#5300=ORIENTED_EDGE('',*,*,#3788,.T.);
#5301=ORIENTED_EDGE('',*,*,#3890,.T.);
#5302=ORIENTED_EDGE('',*,*,#3873,.T.);
#5303=ORIENTED_EDGE('',*,*,#3891,.T.);
#5304=ORIENTED_EDGE('',*,*,#3871,.T.);
#5305=ORIENTED_EDGE('',*,*,#3892,.T.);
#5306=ORIENTED_EDGE('',*,*,#3869,.T.);
#5307=ORIENTED_EDGE('',*,*,#3893,.T.);
#5308=ORIENTED_EDGE('',*,*,#3786,.T.);
#5309=ORIENTED_EDGE('',*,*,#3894,.T.);
#5310=ORIENTED_EDGE('',*,*,#3870,.T.);
#5311=ORIENTED_EDGE('',*,*,#3895,.T.);
#5312=ORIENTED_EDGE('',*,*,#3889,.F.);
#5313=ORIENTED_EDGE('',*,*,#3886,.F.);
#5314=ORIENTED_EDGE('',*,*,#3879,.F.);
#5315=ORIENTED_EDGE('',*,*,#3791,.F.);
#5316=ORIENTED_EDGE('',*,*,#3705,.T.);
#5317=ORIENTED_EDGE('',*,*,#3793,.F.);
#5318=ORIENTED_EDGE('',*,*,#3880,.F.);
#5319=ORIENTED_EDGE('',*,*,#3877,.F.);
#5320=ORIENTED_EDGE('',*,*,#3894,.F.);
#5321=ORIENTED_EDGE('',*,*,#3785,.F.);
#5322=ORIENTED_EDGE('',*,*,#3721,.T.);
#5323=ORIENTED_EDGE('',*,*,#3734,.T.);
#5324=ORIENTED_EDGE('',*,*,#3885,.F.);
#5325=ORIENTED_EDGE('',*,*,#3893,.F.);
#5326=ORIENTED_EDGE('',*,*,#3878,.F.);
#5327=ORIENTED_EDGE('',*,*,#3887,.F.);
#5328=ORIENTED_EDGE('',*,*,#3695,.T.);
#5329=ORIENTED_EDGE('',*,*,#3691,.T.);
#5330=ORIENTED_EDGE('',*,*,#3688,.T.);
#5331=ORIENTED_EDGE('',*,*,#3686,.T.);
#5332=ORIENTED_EDGE('',*,*,#3684,.T.);
#5333=ORIENTED_EDGE('',*,*,#3681,.T.);
#5334=ORIENTED_EDGE('',*,*,#3890,.F.);
#5335=ORIENTED_EDGE('',*,*,#3787,.F.);
#5336=ORIENTED_EDGE('',*,*,#3895,.F.);
#5337=ORIENTED_EDGE('',*,*,#3892,.F.);
#5338=ORIENTED_EDGE('',*,*,#3888,.F.);
#5339=ORIENTED_EDGE('',*,*,#3789,.F.);
#5340=ORIENTED_EDGE('',*,*,#3891,.F.);
#5341=ORIENTED_EDGE('',*,*,#3884,.F.);
#5342=ORIENTED_EDGE('',*,*,#3896,.T.);
#5343=ORIENTED_EDGE('',*,*,#3897,.T.);
#5344=ORIENTED_EDGE('',*,*,#3898,.T.);
#5345=ORIENTED_EDGE('',*,*,#3899,.F.);
#5346=ORIENTED_EDGE('',*,*,#3900,.T.);
#5347=ORIENTED_EDGE('',*,*,#3901,.T.);
#5348=ORIENTED_EDGE('',*,*,#3902,.T.);
#5349=ORIENTED_EDGE('',*,*,#3903,.F.);
#5350=ORIENTED_EDGE('',*,*,#3904,.T.);
#5351=ORIENTED_EDGE('',*,*,#3905,.T.);
#5352=ORIENTED_EDGE('',*,*,#3906,.T.);
#5353=ORIENTED_EDGE('',*,*,#3907,.F.);
#5354=ORIENTED_EDGE('',*,*,#3908,.T.);
#5355=ORIENTED_EDGE('',*,*,#3909,.F.);
#5356=ORIENTED_EDGE('',*,*,#3908,.F.);
#5357=ORIENTED_EDGE('',*,*,#3910,.F.);
#5358=ORIENTED_EDGE('',*,*,#3911,.T.);
#5359=ORIENTED_EDGE('',*,*,#3905,.F.);
#5360=ORIENTED_EDGE('',*,*,#3911,.F.);
#5361=ORIENTED_EDGE('',*,*,#3912,.F.);
#5362=ORIENTED_EDGE('',*,*,#3913,.T.);
#5363=ORIENTED_EDGE('',*,*,#3904,.F.);
#5364=ORIENTED_EDGE('',*,*,#3913,.F.);
#5365=ORIENTED_EDGE('',*,*,#3914,.F.);
#5366=ORIENTED_EDGE('',*,*,#3915,.T.);
#5367=ORIENTED_EDGE('',*,*,#3916,.F.);
#5368=ORIENTED_EDGE('',*,*,#3915,.F.);
#5369=ORIENTED_EDGE('',*,*,#3917,.F.);
#5370=ORIENTED_EDGE('',*,*,#3918,.T.);
#5371=ORIENTED_EDGE('',*,*,#3919,.T.);
#5372=ORIENTED_EDGE('',*,*,#3920,.F.);
#5373=ORIENTED_EDGE('',*,*,#3921,.F.);
#5374=ORIENTED_EDGE('',*,*,#3922,.T.);
#5375=ORIENTED_EDGE('',*,*,#3923,.T.);
#5376=ORIENTED_EDGE('',*,*,#3918,.F.);
#5377=ORIENTED_EDGE('',*,*,#3924,.F.);
#5378=ORIENTED_EDGE('',*,*,#3925,.T.);
#5379=ORIENTED_EDGE('',*,*,#3926,.T.);
#5380=ORIENTED_EDGE('',*,*,#3922,.F.);
#5381=ORIENTED_EDGE('',*,*,#3927,.F.);
#5382=ORIENTED_EDGE('',*,*,#3928,.T.);
#5383=ORIENTED_EDGE('',*,*,#3929,.T.);
#5384=ORIENTED_EDGE('',*,*,#3925,.F.);
#5385=ORIENTED_EDGE('',*,*,#3930,.F.);
#5386=ORIENTED_EDGE('',*,*,#3931,.T.);
#5387=ORIENTED_EDGE('',*,*,#3932,.T.);
#5388=ORIENTED_EDGE('',*,*,#3928,.F.);
#5389=ORIENTED_EDGE('',*,*,#3933,.F.);
#5390=ORIENTED_EDGE('',*,*,#3920,.T.);
#5391=ORIENTED_EDGE('',*,*,#3934,.T.);
#5392=ORIENTED_EDGE('',*,*,#3931,.F.);
#5393=ORIENTED_EDGE('',*,*,#3934,.F.);
#5394=ORIENTED_EDGE('',*,*,#3919,.F.);
#5395=ORIENTED_EDGE('',*,*,#3923,.F.);
#5396=ORIENTED_EDGE('',*,*,#3926,.F.);
#5397=ORIENTED_EDGE('',*,*,#3929,.F.);
#5398=ORIENTED_EDGE('',*,*,#3932,.F.);
#5399=ORIENTED_EDGE('',*,*,#3935,.F.);
#5400=ORIENTED_EDGE('',*,*,#3936,.F.);
#5401=ORIENTED_EDGE('',*,*,#3937,.T.);
#5402=ORIENTED_EDGE('',*,*,#3938,.T.);
#5403=ORIENTED_EDGE('',*,*,#3939,.F.);
#5404=ORIENTED_EDGE('',*,*,#3940,.F.);
#5405=ORIENTED_EDGE('',*,*,#3941,.T.);
#5406=ORIENTED_EDGE('',*,*,#3942,.T.);
#5407=ORIENTED_EDGE('',*,*,#3937,.F.);
#5408=ORIENTED_EDGE('',*,*,#3943,.F.);
#5409=ORIENTED_EDGE('',*,*,#3944,.T.);
#5410=ORIENTED_EDGE('',*,*,#3945,.T.);
#5411=ORIENTED_EDGE('',*,*,#3941,.F.);
#5412=ORIENTED_EDGE('',*,*,#3946,.F.);
#5413=ORIENTED_EDGE('',*,*,#3947,.T.);
#5414=ORIENTED_EDGE('',*,*,#3948,.T.);
#5415=ORIENTED_EDGE('',*,*,#3944,.F.);
#5416=ORIENTED_EDGE('',*,*,#3949,.F.);
#5417=ORIENTED_EDGE('',*,*,#3950,.T.);
#5418=ORIENTED_EDGE('',*,*,#3951,.T.);
#5419=ORIENTED_EDGE('',*,*,#3947,.F.);
#5420=ORIENTED_EDGE('',*,*,#3952,.F.);
#5421=ORIENTED_EDGE('',*,*,#3939,.T.);
#5422=ORIENTED_EDGE('',*,*,#3953,.T.);
#5423=ORIENTED_EDGE('',*,*,#3950,.F.);
#5424=ORIENTED_EDGE('',*,*,#3953,.F.);
#5425=ORIENTED_EDGE('',*,*,#3938,.F.);
#5426=ORIENTED_EDGE('',*,*,#3942,.F.);
#5427=ORIENTED_EDGE('',*,*,#3945,.F.);
#5428=ORIENTED_EDGE('',*,*,#3948,.F.);
#5429=ORIENTED_EDGE('',*,*,#3951,.F.);
#5430=ORIENTED_EDGE('',*,*,#3954,.F.);
#5431=ORIENTED_EDGE('',*,*,#3954,.T.);
#5432=ORIENTED_EDGE('',*,*,#3955,.T.);
#5433=ORIENTED_EDGE('',*,*,#3956,.F.);
#5434=ORIENTED_EDGE('',*,*,#3955,.F.);
#5435=ORIENTED_EDGE('',*,*,#3935,.T.);
#5436=ORIENTED_EDGE('',*,*,#3957,.T.);
#5437=ORIENTED_EDGE('',*,*,#3958,.F.);
#5438=ORIENTED_EDGE('',*,*,#3957,.F.);
#5439=ORIENTED_EDGE('',*,*,#3959,.F.);
#5440=ORIENTED_EDGE('',*,*,#3960,.F.);
#5441=ORIENTED_EDGE('',*,*,#3961,.F.);
#5442=ORIENTED_EDGE('',*,*,#3962,.T.);
#5443=ORIENTED_EDGE('',*,*,#3963,.F.);
#5444=ORIENTED_EDGE('',*,*,#3964,.T.);
#5445=ORIENTED_EDGE('',*,*,#3965,.F.);
#5446=ORIENTED_EDGE('',*,*,#3966,.F.);
#5447=ORIENTED_EDGE('',*,*,#3967,.F.);
#5448=ORIENTED_EDGE('',*,*,#3968,.T.);
#5449=ORIENTED_EDGE('',*,*,#3969,.F.);
#5450=ORIENTED_EDGE('',*,*,#3970,.F.);
#5451=ORIENTED_EDGE('',*,*,#3971,.F.);
#5452=ORIENTED_EDGE('',*,*,#3972,.T.);
#5453=ORIENTED_EDGE('',*,*,#3973,.F.);
#5454=ORIENTED_EDGE('',*,*,#3974,.F.);
#5455=ORIENTED_EDGE('',*,*,#3975,.F.);
#5456=ORIENTED_EDGE('',*,*,#3976,.T.);
#5457=ORIENTED_EDGE('',*,*,#3977,.F.);
#5458=ORIENTED_EDGE('',*,*,#3978,.F.);
#5459=ORIENTED_EDGE('',*,*,#3979,.F.);
#5460=ORIENTED_EDGE('',*,*,#3980,.F.);
#5461=ORIENTED_EDGE('',*,*,#3981,.F.);
#5462=ORIENTED_EDGE('',*,*,#3982,.T.);
#5463=ORIENTED_EDGE('',*,*,#3983,.F.);
#5464=ORIENTED_EDGE('',*,*,#3984,.F.);
#5465=ORIENTED_EDGE('',*,*,#3985,.F.);
#5466=ORIENTED_EDGE('',*,*,#3986,.T.);
#5467=ORIENTED_EDGE('',*,*,#3987,.F.);
#5468=ORIENTED_EDGE('',*,*,#3956,.T.);
#5469=ORIENTED_EDGE('',*,*,#3988,.F.);
#5470=ORIENTED_EDGE('',*,*,#3958,.T.);
#5471=ORIENTED_EDGE('',*,*,#3989,.F.);
#5472=ORIENTED_EDGE('',*,*,#3962,.F.);
#5473=ORIENTED_EDGE('',*,*,#3990,.F.);
#5474=ORIENTED_EDGE('',*,*,#3976,.F.);
#5475=ORIENTED_EDGE('',*,*,#3991,.F.);
#5476=ORIENTED_EDGE('',*,*,#3982,.F.);
#5477=ORIENTED_EDGE('',*,*,#3992,.F.);
#5478=ORIENTED_EDGE('',*,*,#3964,.F.);
#5479=ORIENTED_EDGE('',*,*,#3993,.F.);
#5480=ORIENTED_EDGE('',*,*,#3986,.F.);
#5481=ORIENTED_EDGE('',*,*,#3994,.F.);
#5482=ORIENTED_EDGE('',*,*,#3968,.F.);
#5483=ORIENTED_EDGE('',*,*,#3995,.F.);
#5484=ORIENTED_EDGE('',*,*,#3996,.F.);
#5485=ORIENTED_EDGE('',*,*,#3997,.F.);
#5486=ORIENTED_EDGE('',*,*,#3972,.F.);
#5487=ORIENTED_EDGE('',*,*,#3998,.F.);
#5488=ORIENTED_EDGE('',*,*,#3999,.F.);
#5489=ORIENTED_EDGE('',*,*,#4000,.F.);
#5490=ORIENTED_EDGE('',*,*,#3996,.T.);
#5491=ORIENTED_EDGE('',*,*,#4001,.T.);
#5492=ORIENTED_EDGE('',*,*,#4002,.F.);
#5493=ORIENTED_EDGE('',*,*,#4003,.F.);
#5494=ORIENTED_EDGE('',*,*,#4004,.F.);
#5495=ORIENTED_EDGE('',*,*,#4005,.F.);
#5496=ORIENTED_EDGE('',*,*,#4006,.F.);
#5497=ORIENTED_EDGE('',*,*,#3973,.T.);
#5498=ORIENTED_EDGE('',*,*,#3997,.T.);
#5499=ORIENTED_EDGE('',*,*,#4000,.T.);
#5500=ORIENTED_EDGE('',*,*,#4007,.T.);
#5501=ORIENTED_EDGE('',*,*,#4008,.F.);
#5502=ORIENTED_EDGE('',*,*,#4009,.F.);
#5503=ORIENTED_EDGE('',*,*,#4010,.F.);
#5504=ORIENTED_EDGE('',*,*,#4011,.F.);
#5505=ORIENTED_EDGE('',*,*,#4012,.F.);
#5506=ORIENTED_EDGE('',*,*,#4013,.T.);
#5507=ORIENTED_EDGE('',*,*,#3969,.T.);
#5508=ORIENTED_EDGE('',*,*,#3994,.T.);
#5509=ORIENTED_EDGE('',*,*,#3985,.T.);
#5510=ORIENTED_EDGE('',*,*,#4014,.T.);
#5511=ORIENTED_EDGE('',*,*,#4015,.F.);
#5512=ORIENTED_EDGE('',*,*,#4016,.F.);
#5513=ORIENTED_EDGE('',*,*,#4017,.F.);
#5514=ORIENTED_EDGE('',*,*,#4018,.F.);
#5515=ORIENTED_EDGE('',*,*,#4019,.F.);
#5516=ORIENTED_EDGE('',*,*,#4020,.T.);
#5517=ORIENTED_EDGE('',*,*,#3965,.T.);
#5518=ORIENTED_EDGE('',*,*,#3992,.T.);
#5519=ORIENTED_EDGE('',*,*,#3981,.T.);
#5520=ORIENTED_EDGE('',*,*,#4021,.T.);
#5521=ORIENTED_EDGE('',*,*,#4022,.F.);
#5522=ORIENTED_EDGE('',*,*,#4023,.F.);
#5523=ORIENTED_EDGE('',*,*,#3901,.F.);
#5524=ORIENTED_EDGE('',*,*,#4024,.F.);
#5525=ORIENTED_EDGE('',*,*,#4025,.F.);
#5526=ORIENTED_EDGE('',*,*,#4026,.T.);
#5527=ORIENTED_EDGE('',*,*,#3959,.T.);
#5528=ORIENTED_EDGE('',*,*,#3989,.T.);
#5529=ORIENTED_EDGE('',*,*,#3975,.T.);
#5530=ORIENTED_EDGE('',*,*,#4027,.F.);
#5531=ORIENTED_EDGE('',*,*,#4028,.T.);
#5532=ORIENTED_EDGE('',*,*,#4029,.T.);
#5533=ORIENTED_EDGE('',*,*,#4030,.T.);
#5534=ORIENTED_EDGE('',*,*,#4031,.F.);
#5535=ORIENTED_EDGE('',*,*,#3974,.T.);
#5536=ORIENTED_EDGE('',*,*,#4013,.F.);
#5537=ORIENTED_EDGE('',*,*,#4032,.T.);
#5538=ORIENTED_EDGE('',*,*,#4001,.F.);
#5539=ORIENTED_EDGE('',*,*,#4033,.T.);
#5540=ORIENTED_EDGE('',*,*,#4007,.F.);
#5541=ORIENTED_EDGE('',*,*,#3999,.T.);
#5542=ORIENTED_EDGE('',*,*,#4034,.F.);
#5543=ORIENTED_EDGE('',*,*,#4035,.T.);
#5544=ORIENTED_EDGE('',*,*,#4014,.F.);
#5545=ORIENTED_EDGE('',*,*,#3984,.T.);
#5546=ORIENTED_EDGE('',*,*,#4036,.F.);
#5547=ORIENTED_EDGE('',*,*,#4037,.T.);
#5548=ORIENTED_EDGE('',*,*,#4021,.F.);
#5549=ORIENTED_EDGE('',*,*,#3980,.T.);
#5550=ORIENTED_EDGE('',*,*,#4038,.F.);
#5551=ORIENTED_EDGE('',*,*,#4039,.T.);
#5552=ORIENTED_EDGE('',*,*,#4040,.T.);
#5553=ORIENTED_EDGE('',*,*,#4027,.T.);
#5554=ORIENTED_EDGE('',*,*,#3978,.T.);
#5555=ORIENTED_EDGE('',*,*,#4041,.T.);
#5556=ORIENTED_EDGE('',*,*,#4042,.F.);
#5557=ORIENTED_EDGE('',*,*,#4043,.T.);
#5558=ORIENTED_EDGE('',*,*,#4044,.F.);
#5559=ORIENTED_EDGE('',*,*,#4045,.T.);
#5560=ORIENTED_EDGE('',*,*,#4046,.F.);
#5561=ORIENTED_EDGE('',*,*,#4047,.T.);
#5562=ORIENTED_EDGE('',*,*,#4048,.F.);
#5563=ORIENTED_EDGE('',*,*,#4049,.T.);
#5564=ORIENTED_EDGE('',*,*,#3960,.T.);
#5565=ORIENTED_EDGE('',*,*,#4031,.T.);
#5566=ORIENTED_EDGE('',*,*,#4050,.T.);
#5567=ORIENTED_EDGE('',*,*,#4051,.T.);
#5568=ORIENTED_EDGE('',*,*,#4052,.F.);
#5569=ORIENTED_EDGE('',*,*,#3966,.T.);
#5570=ORIENTED_EDGE('',*,*,#4026,.F.);
#5571=ORIENTED_EDGE('',*,*,#4053,.T.);
#5572=ORIENTED_EDGE('',*,*,#4054,.F.);
#5573=ORIENTED_EDGE('',*,*,#3970,.T.);
#5574=ORIENTED_EDGE('',*,*,#4020,.F.);
#5575=ORIENTED_EDGE('',*,*,#4055,.T.);
#5576=ORIENTED_EDGE('',*,*,#4056,.F.);
#5577=ORIENTED_EDGE('',*,*,#4057,.T.);
#5578=ORIENTED_EDGE('',*,*,#4058,.T.);
#5579=ORIENTED_EDGE('',*,*,#4059,.T.);
#5580=ORIENTED_EDGE('',*,*,#4060,.T.);
#5581=ORIENTED_EDGE('',*,*,#4061,.T.);
#5582=ORIENTED_EDGE('',*,*,#4062,.F.);
#5583=ORIENTED_EDGE('',*,*,#4063,.F.);
#5584=ORIENTED_EDGE('',*,*,#4064,.T.);
#5585=ORIENTED_EDGE('',*,*,#3988,.T.);
#5586=ORIENTED_EDGE('',*,*,#4064,.F.);
#5587=ORIENTED_EDGE('',*,*,#3906,.F.);
#5588=ORIENTED_EDGE('',*,*,#4065,.T.);
#5589=ORIENTED_EDGE('',*,*,#3987,.T.);
#5590=ORIENTED_EDGE('',*,*,#4065,.F.);
#5591=ORIENTED_EDGE('',*,*,#4066,.F.);
#5592=ORIENTED_EDGE('',*,*,#4062,.T.);
#5593=ORIENTED_EDGE('',*,*,#4067,.F.);
#5594=ORIENTED_EDGE('',*,*,#4068,.F.);
#5595=ORIENTED_EDGE('',*,*,#4069,.F.);
#5596=ORIENTED_EDGE('',*,*,#4070,.F.);
#5597=ORIENTED_EDGE('',*,*,#4002,.T.);
#5598=ORIENTED_EDGE('',*,*,#4032,.F.);
#5599=ORIENTED_EDGE('',*,*,#4012,.T.);
#5600=ORIENTED_EDGE('',*,*,#4071,.T.);
#5601=ORIENTED_EDGE('',*,*,#4066,.T.);
#5602=ORIENTED_EDGE('',*,*,#4072,.T.);
#5603=ORIENTED_EDGE('',*,*,#4073,.T.);
#5604=ORIENTED_EDGE('',*,*,#4057,.F.);
#5605=ORIENTED_EDGE('',*,*,#4003,.T.);
#5606=ORIENTED_EDGE('',*,*,#4071,.F.);
#5607=ORIENTED_EDGE('',*,*,#4011,.T.);
#5608=ORIENTED_EDGE('',*,*,#4074,.F.);
#5609=ORIENTED_EDGE('',*,*,#4070,.T.);
#5610=ORIENTED_EDGE('',*,*,#4075,.F.);
#5611=ORIENTED_EDGE('',*,*,#4076,.F.);
#5612=ORIENTED_EDGE('',*,*,#4072,.F.);
#5613=ORIENTED_EDGE('',*,*,#4004,.T.);
#5614=ORIENTED_EDGE('',*,*,#4074,.T.);
#5615=ORIENTED_EDGE('',*,*,#4010,.T.);
#5616=ORIENTED_EDGE('',*,*,#4077,.T.);
#5617=ORIENTED_EDGE('',*,*,#3909,.T.);
#5618=ORIENTED_EDGE('',*,*,#3916,.T.);
#5619=ORIENTED_EDGE('',*,*,#4063,.T.);
#5620=ORIENTED_EDGE('',*,*,#4069,.T.);
#5621=ORIENTED_EDGE('',*,*,#4078,.T.);
#5622=ORIENTED_EDGE('',*,*,#4079,.T.);
#5623=ORIENTED_EDGE('',*,*,#4075,.T.);
#5624=ORIENTED_EDGE('',*,*,#4005,.T.);
#5625=ORIENTED_EDGE('',*,*,#4077,.F.);
#5626=ORIENTED_EDGE('',*,*,#4009,.T.);
#5627=ORIENTED_EDGE('',*,*,#4080,.F.);
#5628=ORIENTED_EDGE('',*,*,#4006,.T.);
#5629=ORIENTED_EDGE('',*,*,#4080,.T.);
#5630=ORIENTED_EDGE('',*,*,#4008,.T.);
#5631=ORIENTED_EDGE('',*,*,#4033,.F.);
#5632=ORIENTED_EDGE('',*,*,#4067,.T.);
#5633=ORIENTED_EDGE('',*,*,#4061,.F.);
#5634=ORIENTED_EDGE('',*,*,#4081,.T.);
#5635=ORIENTED_EDGE('',*,*,#4082,.T.);
#5636=ORIENTED_EDGE('',*,*,#3971,.T.);
#5637=ORIENTED_EDGE('',*,*,#4056,.T.);
#5638=ORIENTED_EDGE('',*,*,#4083,.F.);
#5639=ORIENTED_EDGE('',*,*,#4084,.F.);
#5640=ORIENTED_EDGE('',*,*,#4085,.F.);
#5641=ORIENTED_EDGE('',*,*,#4086,.F.);
#5642=ORIENTED_EDGE('',*,*,#4087,.F.);
#5643=ORIENTED_EDGE('',*,*,#4034,.T.);
#5644=ORIENTED_EDGE('',*,*,#3998,.T.);
#5645=ORIENTED_EDGE('',*,*,#3995,.T.);
#5646=ORIENTED_EDGE('',*,*,#4083,.T.);
#5647=ORIENTED_EDGE('',*,*,#4055,.F.);
#5648=ORIENTED_EDGE('',*,*,#4019,.T.);
#5649=ORIENTED_EDGE('',*,*,#4088,.T.);
#5650=ORIENTED_EDGE('',*,*,#4084,.T.);
#5651=ORIENTED_EDGE('',*,*,#4088,.F.);
#5652=ORIENTED_EDGE('',*,*,#4018,.T.);
#5653=ORIENTED_EDGE('',*,*,#4089,.F.);
#5654=ORIENTED_EDGE('',*,*,#4085,.T.);
#5655=ORIENTED_EDGE('',*,*,#4089,.T.);
#5656=ORIENTED_EDGE('',*,*,#4017,.T.);
#5657=ORIENTED_EDGE('',*,*,#4090,.T.);
#5658=ORIENTED_EDGE('',*,*,#4086,.T.);
#5659=ORIENTED_EDGE('',*,*,#4090,.F.);
#5660=ORIENTED_EDGE('',*,*,#4016,.T.);
#5661=ORIENTED_EDGE('',*,*,#4091,.F.);
#5662=ORIENTED_EDGE('',*,*,#4087,.T.);
#5663=ORIENTED_EDGE('',*,*,#4091,.T.);
#5664=ORIENTED_EDGE('',*,*,#4015,.T.);
#5665=ORIENTED_EDGE('',*,*,#4035,.F.);
#5666=ORIENTED_EDGE('',*,*,#3967,.T.);
#5667=ORIENTED_EDGE('',*,*,#4054,.T.);
#5668=ORIENTED_EDGE('',*,*,#4092,.F.);
#5669=ORIENTED_EDGE('',*,*,#4093,.F.);
#5670=ORIENTED_EDGE('',*,*,#3897,.F.);
#5671=ORIENTED_EDGE('',*,*,#4094,.F.);
#5672=ORIENTED_EDGE('',*,*,#4095,.F.);
#5673=ORIENTED_EDGE('',*,*,#4036,.T.);
#5674=ORIENTED_EDGE('',*,*,#3983,.T.);
#5675=ORIENTED_EDGE('',*,*,#3993,.T.);
#5676=ORIENTED_EDGE('',*,*,#4092,.T.);
#5677=ORIENTED_EDGE('',*,*,#4053,.F.);
#5678=ORIENTED_EDGE('',*,*,#4025,.T.);
#5679=ORIENTED_EDGE('',*,*,#4096,.T.);
#5680=ORIENTED_EDGE('',*,*,#3899,.T.);
#5681=ORIENTED_EDGE('',*,*,#3898,.F.);
#5682=ORIENTED_EDGE('',*,*,#4093,.T.);
#5683=ORIENTED_EDGE('',*,*,#4096,.F.);
#5684=ORIENTED_EDGE('',*,*,#4024,.T.);
#5685=ORIENTED_EDGE('',*,*,#3900,.F.);
#5686=ORIENTED_EDGE('',*,*,#3903,.T.);
#5687=ORIENTED_EDGE('',*,*,#3902,.F.);
#5688=ORIENTED_EDGE('',*,*,#4023,.T.);
#5689=ORIENTED_EDGE('',*,*,#4097,.F.);
#5690=ORIENTED_EDGE('',*,*,#4094,.T.);
#5691=ORIENTED_EDGE('',*,*,#3896,.F.);
#5692=ORIENTED_EDGE('',*,*,#4095,.T.);
#5693=ORIENTED_EDGE('',*,*,#4097,.T.);
#5694=ORIENTED_EDGE('',*,*,#4022,.T.);
#5695=ORIENTED_EDGE('',*,*,#4037,.F.);
#5696=ORIENTED_EDGE('',*,*,#3963,.T.);
#5697=ORIENTED_EDGE('',*,*,#4052,.T.);
#5698=ORIENTED_EDGE('',*,*,#4098,.F.);
#5699=ORIENTED_EDGE('',*,*,#4099,.F.);
#5700=ORIENTED_EDGE('',*,*,#4100,.F.);
#5701=ORIENTED_EDGE('',*,*,#4101,.F.);
#5702=ORIENTED_EDGE('',*,*,#4102,.F.);
#5703=ORIENTED_EDGE('',*,*,#4038,.T.);
#5704=ORIENTED_EDGE('',*,*,#3979,.T.);
#5705=ORIENTED_EDGE('',*,*,#3991,.T.);
#5706=ORIENTED_EDGE('',*,*,#4098,.T.);
#5707=ORIENTED_EDGE('',*,*,#4051,.F.);
#5708=ORIENTED_EDGE('',*,*,#4103,.T.);
#5709=ORIENTED_EDGE('',*,*,#4104,.T.);
#5710=ORIENTED_EDGE('',*,*,#4099,.T.);
#5711=ORIENTED_EDGE('',*,*,#4104,.F.);
#5712=ORIENTED_EDGE('',*,*,#4105,.F.);
#5713=ORIENTED_EDGE('',*,*,#4106,.F.);
#5714=ORIENTED_EDGE('',*,*,#4100,.T.);
#5715=ORIENTED_EDGE('',*,*,#4106,.T.);
#5716=ORIENTED_EDGE('',*,*,#4107,.T.);
#5717=ORIENTED_EDGE('',*,*,#4108,.T.);
#5718=ORIENTED_EDGE('',*,*,#4102,.T.);
#5719=ORIENTED_EDGE('',*,*,#4109,.T.);
#5720=ORIENTED_EDGE('',*,*,#4110,.T.);
#5721=ORIENTED_EDGE('',*,*,#4039,.F.);
#5722=ORIENTED_EDGE('',*,*,#4101,.T.);
#5723=ORIENTED_EDGE('',*,*,#4108,.F.);
#5724=ORIENTED_EDGE('',*,*,#4111,.F.);
#5725=ORIENTED_EDGE('',*,*,#4109,.F.);
#5726=ORIENTED_EDGE('',*,*,#4112,.T.);
#5727=ORIENTED_EDGE('',*,*,#4113,.T.);
#5728=ORIENTED_EDGE('',*,*,#4111,.T.);
#5729=ORIENTED_EDGE('',*,*,#4114,.T.);
#5730=ORIENTED_EDGE('',*,*,#4115,.T.);
#5731=ORIENTED_EDGE('',*,*,#4116,.T.);
#5732=ORIENTED_EDGE('',*,*,#4105,.T.);
#5733=ORIENTED_EDGE('',*,*,#4117,.T.);
#5734=ORIENTED_EDGE('',*,*,#4118,.T.);
#5735=ORIENTED_EDGE('',*,*,#4112,.F.);
#5736=ORIENTED_EDGE('',*,*,#4107,.F.);
#5737=ORIENTED_EDGE('',*,*,#4118,.F.);
#5738=ORIENTED_EDGE('',*,*,#4029,.F.);
#5739=ORIENTED_EDGE('',*,*,#4050,.F.);
#5740=ORIENTED_EDGE('',*,*,#4030,.F.);
#5741=ORIENTED_EDGE('',*,*,#4117,.F.);
#5742=ORIENTED_EDGE('',*,*,#4103,.F.);
#5743=ORIENTED_EDGE('',*,*,#4119,.T.);
#5744=ORIENTED_EDGE('',*,*,#4076,.T.);
#5745=ORIENTED_EDGE('',*,*,#4120,.T.);
#5746=ORIENTED_EDGE('',*,*,#4120,.F.);
#5747=ORIENTED_EDGE('',*,*,#4079,.F.);
#5748=ORIENTED_EDGE('',*,*,#4116,.F.);
#5749=ORIENTED_EDGE('',*,*,#4121,.F.);
#5750=ORIENTED_EDGE('',*,*,#4058,.F.);
#5751=ORIENTED_EDGE('',*,*,#4073,.F.);
#5752=ORIENTED_EDGE('',*,*,#4119,.F.);
#5753=ORIENTED_EDGE('',*,*,#4122,.F.);
#5754=ORIENTED_EDGE('',*,*,#4060,.F.);
#5755=ORIENTED_EDGE('',*,*,#4123,.F.);
#5756=ORIENTED_EDGE('',*,*,#4115,.F.);
#5757=ORIENTED_EDGE('',*,*,#4081,.F.);
#5758=ORIENTED_EDGE('',*,*,#4068,.T.);
#5759=ORIENTED_EDGE('',*,*,#4082,.F.);
#5760=ORIENTED_EDGE('',*,*,#4114,.F.);
#5761=ORIENTED_EDGE('',*,*,#4078,.F.);
#5762=ORIENTED_EDGE('',*,*,#4040,.F.);
#5763=ORIENTED_EDGE('',*,*,#4110,.F.);
#5764=ORIENTED_EDGE('',*,*,#4113,.F.);
#5765=ORIENTED_EDGE('',*,*,#4028,.F.);
#5766=ORIENTED_EDGE('',*,*,#4122,.T.);
#5767=ORIENTED_EDGE('',*,*,#4121,.T.);
#5768=ORIENTED_EDGE('',*,*,#4123,.T.);
#5769=ORIENTED_EDGE('',*,*,#4059,.F.);
#5770=ORIENTED_EDGE('',*,*,#4124,.F.);
#5771=ORIENTED_EDGE('',*,*,#4125,.F.);
#5772=ORIENTED_EDGE('',*,*,#4126,.F.);
#5773=ORIENTED_EDGE('',*,*,#4127,.F.);
#5774=ORIENTED_EDGE('',*,*,#4128,.F.);
#5775=ORIENTED_EDGE('',*,*,#4129,.F.);
#5776=ORIENTED_EDGE('',*,*,#4130,.F.);
#5777=ORIENTED_EDGE('',*,*,#4131,.F.);
#5778=ORIENTED_EDGE('',*,*,#4132,.F.);
#5779=ORIENTED_EDGE('',*,*,#4124,.T.);
#5780=ORIENTED_EDGE('',*,*,#4133,.T.);
#5781=ORIENTED_EDGE('',*,*,#4131,.T.);
#5782=ORIENTED_EDGE('',*,*,#4134,.T.);
#5783=ORIENTED_EDGE('',*,*,#4048,.T.);
#5784=ORIENTED_EDGE('',*,*,#4135,.T.);
#5785=ORIENTED_EDGE('',*,*,#4132,.T.);
#5786=ORIENTED_EDGE('',*,*,#4136,.T.);
#5787=ORIENTED_EDGE('',*,*,#4137,.F.);
#5788=ORIENTED_EDGE('',*,*,#4138,.F.);
#5789=ORIENTED_EDGE('',*,*,#4139,.F.);
#5790=ORIENTED_EDGE('',*,*,#4138,.T.);
#5791=ORIENTED_EDGE('',*,*,#4140,.T.);
#5792=ORIENTED_EDGE('',*,*,#4128,.T.);
#5793=ORIENTED_EDGE('',*,*,#4141,.T.);
#5794=ORIENTED_EDGE('',*,*,#4130,.T.);
#5795=ORIENTED_EDGE('',*,*,#4142,.T.);
#5796=ORIENTED_EDGE('',*,*,#4139,.T.);
#5797=ORIENTED_EDGE('',*,*,#4143,.T.);
#5798=ORIENTED_EDGE('',*,*,#4046,.T.);
#5799=ORIENTED_EDGE('',*,*,#4144,.T.);
#5800=ORIENTED_EDGE('',*,*,#4137,.T.);
#5801=ORIENTED_EDGE('',*,*,#4145,.T.);
#5802=ORIENTED_EDGE('',*,*,#4044,.T.);
#5803=ORIENTED_EDGE('',*,*,#4146,.T.);
#5804=ORIENTED_EDGE('',*,*,#4129,.T.);
#5805=ORIENTED_EDGE('',*,*,#4147,.T.);
#5806=ORIENTED_EDGE('',*,*,#4127,.T.);
#5807=ORIENTED_EDGE('',*,*,#4148,.T.);
#5808=ORIENTED_EDGE('',*,*,#4125,.T.);
#5809=ORIENTED_EDGE('',*,*,#4149,.T.);
#5810=ORIENTED_EDGE('',*,*,#4042,.T.);
#5811=ORIENTED_EDGE('',*,*,#4150,.T.);
#5812=ORIENTED_EDGE('',*,*,#4126,.T.);
#5813=ORIENTED_EDGE('',*,*,#4151,.T.);
#5814=ORIENTED_EDGE('',*,*,#4145,.F.);
#5815=ORIENTED_EDGE('',*,*,#4142,.F.);
#5816=ORIENTED_EDGE('',*,*,#4135,.F.);
#5817=ORIENTED_EDGE('',*,*,#4047,.F.);
#5818=ORIENTED_EDGE('',*,*,#3961,.T.);
#5819=ORIENTED_EDGE('',*,*,#4049,.F.);
#5820=ORIENTED_EDGE('',*,*,#4136,.F.);
#5821=ORIENTED_EDGE('',*,*,#4133,.F.);
#5822=ORIENTED_EDGE('',*,*,#4150,.F.);
#5823=ORIENTED_EDGE('',*,*,#4041,.F.);
#5824=ORIENTED_EDGE('',*,*,#3977,.T.);
#5825=ORIENTED_EDGE('',*,*,#3990,.T.);
#5826=ORIENTED_EDGE('',*,*,#4141,.F.);
#5827=ORIENTED_EDGE('',*,*,#4149,.F.);
#5828=ORIENTED_EDGE('',*,*,#4134,.F.);
#5829=ORIENTED_EDGE('',*,*,#4143,.F.);
#5830=ORIENTED_EDGE('',*,*,#3936,.T.);
#5831=ORIENTED_EDGE('',*,*,#3952,.T.);
#5832=ORIENTED_EDGE('',*,*,#3949,.T.);
#5833=ORIENTED_EDGE('',*,*,#3946,.T.);
#5834=ORIENTED_EDGE('',*,*,#3943,.T.);
#5835=ORIENTED_EDGE('',*,*,#3940,.T.);
#5836=ORIENTED_EDGE('',*,*,#3917,.T.);
#5837=ORIENTED_EDGE('',*,*,#3933,.T.);
#5838=ORIENTED_EDGE('',*,*,#3930,.T.);
#5839=ORIENTED_EDGE('',*,*,#3927,.T.);
#5840=ORIENTED_EDGE('',*,*,#3924,.T.);
#5841=ORIENTED_EDGE('',*,*,#3921,.T.);
#5842=ORIENTED_EDGE('',*,*,#3914,.T.);
#5843=ORIENTED_EDGE('',*,*,#3912,.T.);
#5844=ORIENTED_EDGE('',*,*,#3910,.T.);
#5845=ORIENTED_EDGE('',*,*,#3907,.T.);
#5846=ORIENTED_EDGE('',*,*,#4146,.F.);
#5847=ORIENTED_EDGE('',*,*,#4043,.F.);
#5848=ORIENTED_EDGE('',*,*,#4151,.F.);
#5849=ORIENTED_EDGE('',*,*,#4148,.F.);
#5850=ORIENTED_EDGE('',*,*,#4144,.F.);
#5851=ORIENTED_EDGE('',*,*,#4045,.F.);
#5852=ORIENTED_EDGE('',*,*,#4147,.F.);
#5853=ORIENTED_EDGE('',*,*,#4140,.F.);
#5854=ORIENTED_EDGE('',*,*,#4152,.F.);
#5855=ORIENTED_EDGE('',*,*,#4153,.T.);
#5856=ORIENTED_EDGE('',*,*,#4154,.F.);
#5857=ORIENTED_EDGE('',*,*,#4153,.F.);
#5858=ORIENTED_EDGE('',*,*,#4155,.F.);
#5859=ORIENTED_EDGE('',*,*,#4156,.T.);
#5860=ORIENTED_EDGE('',*,*,#4157,.F.);
#5861=ORIENTED_EDGE('',*,*,#4156,.F.);
#5862=ORIENTED_EDGE('',*,*,#4158,.T.);
#5863=ORIENTED_EDGE('',*,*,#4159,.T.);
#5864=ORIENTED_EDGE('',*,*,#4160,.F.);
#5865=ORIENTED_EDGE('',*,*,#4161,.T.);
#5866=ORIENTED_EDGE('',*,*,#4158,.F.);
#5867=ORIENTED_EDGE('',*,*,#4161,.F.);
#5868=ORIENTED_EDGE('',*,*,#4160,.T.);
#5869=ORIENTED_EDGE('',*,*,#4162,.T.);
#5870=ORIENTED_EDGE('',*,*,#4163,.T.);
#5871=ORIENTED_EDGE('',*,*,#4164,.F.);
#5872=ORIENTED_EDGE('',*,*,#4165,.T.);
#5873=ORIENTED_EDGE('',*,*,#4162,.F.);
#5874=ORIENTED_EDGE('',*,*,#4165,.F.);
#5875=ORIENTED_EDGE('',*,*,#4164,.T.);
#5876=ORIENTED_EDGE('',*,*,#4166,.T.);
#5877=ORIENTED_EDGE('',*,*,#4167,.T.);
#5878=ORIENTED_EDGE('',*,*,#4168,.F.);
#5879=ORIENTED_EDGE('',*,*,#4169,.T.);
#5880=ORIENTED_EDGE('',*,*,#4166,.F.);
#5881=ORIENTED_EDGE('',*,*,#4169,.F.);
#5882=ORIENTED_EDGE('',*,*,#4168,.T.);
#5883=ORIENTED_EDGE('',*,*,#4170,.T.);
#5884=ORIENTED_EDGE('',*,*,#4171,.T.);
#5885=ORIENTED_EDGE('',*,*,#4172,.F.);
#5886=ORIENTED_EDGE('',*,*,#4173,.T.);
#5887=ORIENTED_EDGE('',*,*,#4170,.F.);
#5888=ORIENTED_EDGE('',*,*,#4173,.F.);
#5889=ORIENTED_EDGE('',*,*,#4172,.T.);
#5890=ORIENTED_EDGE('',*,*,#4159,.F.);
#5891=ORIENTED_EDGE('',*,*,#4174,.T.);
#5892=ORIENTED_EDGE('',*,*,#4175,.F.);
#5893=ORIENTED_EDGE('',*,*,#4174,.F.);
#5894=ORIENTED_EDGE('',*,*,#4163,.F.);
#5895=ORIENTED_EDGE('',*,*,#4176,.T.);
#5896=ORIENTED_EDGE('',*,*,#4177,.F.);
#5897=ORIENTED_EDGE('',*,*,#4176,.F.);
#5898=ORIENTED_EDGE('',*,*,#4167,.F.);
#5899=ORIENTED_EDGE('',*,*,#4178,.T.);
#5900=ORIENTED_EDGE('',*,*,#4179,.F.);
#5901=ORIENTED_EDGE('',*,*,#4178,.F.);
#5902=ORIENTED_EDGE('',*,*,#4171,.F.);
#5903=ORIENTED_EDGE('',*,*,#4180,.T.);
#5904=ORIENTED_EDGE('',*,*,#4181,.F.);
#5905=ORIENTED_EDGE('',*,*,#4180,.F.);
#5906=ORIENTED_EDGE('',*,*,#4182,.T.);
#5907=ORIENTED_EDGE('',*,*,#4183,.T.);
#5908=ORIENTED_EDGE('',*,*,#4184,.T.);
#5909=ORIENTED_EDGE('',*,*,#4185,.T.);
#5910=ORIENTED_EDGE('',*,*,#4186,.T.);
#5911=ORIENTED_EDGE('',*,*,#4187,.T.);
#5912=ORIENTED_EDGE('',*,*,#4182,.F.);
#5913=ORIENTED_EDGE('',*,*,#4188,.T.);
#5914=ORIENTED_EDGE('',*,*,#4189,.T.);
#5915=ORIENTED_EDGE('',*,*,#4190,.T.);
#5916=ORIENTED_EDGE('',*,*,#4186,.F.);
#5917=ORIENTED_EDGE('',*,*,#4191,.T.);
#5918=ORIENTED_EDGE('',*,*,#4192,.T.);
#5919=ORIENTED_EDGE('',*,*,#4193,.T.);
#5920=ORIENTED_EDGE('',*,*,#4189,.F.);
#5921=ORIENTED_EDGE('',*,*,#4194,.T.);
#5922=ORIENTED_EDGE('',*,*,#4195,.T.);
#5923=ORIENTED_EDGE('',*,*,#4196,.T.);
#5924=ORIENTED_EDGE('',*,*,#4192,.F.);
#5925=ORIENTED_EDGE('',*,*,#4197,.T.);
#5926=ORIENTED_EDGE('',*,*,#4198,.T.);
#5927=ORIENTED_EDGE('',*,*,#4199,.T.);
#5928=ORIENTED_EDGE('',*,*,#4195,.F.);
#5929=ORIENTED_EDGE('',*,*,#4200,.T.);
#5930=ORIENTED_EDGE('',*,*,#4201,.T.);
#5931=ORIENTED_EDGE('',*,*,#4202,.T.);
#5932=ORIENTED_EDGE('',*,*,#4198,.F.);
#5933=ORIENTED_EDGE('',*,*,#4203,.T.);
#5934=ORIENTED_EDGE('',*,*,#4184,.F.);
#5935=ORIENTED_EDGE('',*,*,#4204,.T.);
#5936=ORIENTED_EDGE('',*,*,#4201,.F.);
#5937=ORIENTED_EDGE('',*,*,#4205,.T.);
#5938=ORIENTED_EDGE('',*,*,#4199,.F.);
#5939=ORIENTED_EDGE('',*,*,#4206,.F.);
#5940=ORIENTED_EDGE('',*,*,#4207,.F.);
#5941=ORIENTED_EDGE('',*,*,#4208,.F.);
#5942=ORIENTED_EDGE('',*,*,#4202,.F.);
#5943=ORIENTED_EDGE('',*,*,#4209,.T.);
#5944=ORIENTED_EDGE('',*,*,#4210,.T.);
#5945=ORIENTED_EDGE('',*,*,#4206,.T.);
#5946=ORIENTED_EDGE('',*,*,#4204,.F.);
#5947=ORIENTED_EDGE('',*,*,#4211,.F.);
#5948=ORIENTED_EDGE('',*,*,#4212,.F.);
#5949=ORIENTED_EDGE('',*,*,#4209,.F.);
#5950=ORIENTED_EDGE('',*,*,#4183,.F.);
#5951=ORIENTED_EDGE('',*,*,#4213,.T.);
#5952=ORIENTED_EDGE('',*,*,#4214,.T.);
#5953=ORIENTED_EDGE('',*,*,#4211,.T.);
#5954=ORIENTED_EDGE('',*,*,#4185,.F.);
#5955=ORIENTED_EDGE('',*,*,#4205,.F.);
#5956=ORIENTED_EDGE('',*,*,#4203,.F.);
#5957=ORIENTED_EDGE('',*,*,#4200,.F.);
#5958=ORIENTED_EDGE('',*,*,#4197,.F.);
#5959=ORIENTED_EDGE('',*,*,#4194,.F.);
#5960=ORIENTED_EDGE('',*,*,#4191,.F.);
#5961=ORIENTED_EDGE('',*,*,#4188,.F.);
#5962=ORIENTED_EDGE('',*,*,#4152,.T.);
#5963=ORIENTED_EDGE('',*,*,#4155,.T.);
#5964=ORIENTED_EDGE('',*,*,#4187,.F.);
#5965=ORIENTED_EDGE('',*,*,#4215,.F.);
#5966=ORIENTED_EDGE('',*,*,#4216,.F.);
#5967=ORIENTED_EDGE('',*,*,#4213,.F.);
#5968=ORIENTED_EDGE('',*,*,#4196,.F.);
#5969=ORIENTED_EDGE('',*,*,#4208,.T.);
#5970=ORIENTED_EDGE('',*,*,#4217,.T.);
#5971=ORIENTED_EDGE('',*,*,#4218,.T.);
#5972=ORIENTED_EDGE('',*,*,#4190,.F.);
#5973=ORIENTED_EDGE('',*,*,#4219,.T.);
#5974=ORIENTED_EDGE('',*,*,#4220,.T.);
#5975=ORIENTED_EDGE('',*,*,#4215,.T.);
#5976=ORIENTED_EDGE('',*,*,#4214,.F.);
#5977=ORIENTED_EDGE('',*,*,#4216,.T.);
#5978=ORIENTED_EDGE('',*,*,#4220,.F.);
#5979=ORIENTED_EDGE('',*,*,#4221,.T.);
#5980=ORIENTED_EDGE('',*,*,#4217,.F.);
#5981=ORIENTED_EDGE('',*,*,#4207,.T.);
#5982=ORIENTED_EDGE('',*,*,#4210,.F.);
#5983=ORIENTED_EDGE('',*,*,#4212,.T.);
#5984=ORIENTED_EDGE('',*,*,#4154,.T.);
#5985=ORIENTED_EDGE('',*,*,#4157,.T.);
#5986=ORIENTED_EDGE('',*,*,#4175,.T.);
#5987=ORIENTED_EDGE('',*,*,#4177,.T.);
#5988=ORIENTED_EDGE('',*,*,#4179,.T.);
#5989=ORIENTED_EDGE('',*,*,#4181,.T.);
#5990=ORIENTED_EDGE('',*,*,#4193,.F.);
#5991=ORIENTED_EDGE('',*,*,#4218,.F.);
#5992=ORIENTED_EDGE('',*,*,#4221,.F.);
#5993=ORIENTED_EDGE('',*,*,#4219,.F.);
#5994=ORIENTED_EDGE('',*,*,#4222,.F.);
#5995=ORIENTED_EDGE('',*,*,#4223,.T.);
#5996=ORIENTED_EDGE('',*,*,#4224,.T.);
#5997=ORIENTED_EDGE('',*,*,#4225,.T.);
#5998=ORIENTED_EDGE('',*,*,#4226,.F.);
#5999=ORIENTED_EDGE('',*,*,#4227,.T.);
#6000=ORIENTED_EDGE('',*,*,#4222,.T.);
#6001=ORIENTED_EDGE('',*,*,#4228,.T.);
#6002=ORIENTED_EDGE('',*,*,#4229,.F.);
#6003=ORIENTED_EDGE('',*,*,#4230,.T.);
#6004=ORIENTED_EDGE('',*,*,#4226,.T.);
#6005=ORIENTED_EDGE('',*,*,#4231,.T.);
#6006=ORIENTED_EDGE('',*,*,#4232,.F.);
#6007=ORIENTED_EDGE('',*,*,#4233,.T.);
#6008=ORIENTED_EDGE('',*,*,#4229,.T.);
#6009=ORIENTED_EDGE('',*,*,#4234,.T.);
#6010=ORIENTED_EDGE('',*,*,#4235,.F.);
#6011=ORIENTED_EDGE('',*,*,#4236,.T.);
#6012=ORIENTED_EDGE('',*,*,#4232,.T.);
#6013=ORIENTED_EDGE('',*,*,#4237,.T.);
#6014=ORIENTED_EDGE('',*,*,#4238,.F.);
#6015=ORIENTED_EDGE('',*,*,#4239,.T.);
#6016=ORIENTED_EDGE('',*,*,#4235,.T.);
#6017=ORIENTED_EDGE('',*,*,#4240,.T.);
#6018=ORIENTED_EDGE('',*,*,#4241,.F.);
#6019=ORIENTED_EDGE('',*,*,#4242,.T.);
#6020=ORIENTED_EDGE('',*,*,#4238,.T.);
#6021=ORIENTED_EDGE('',*,*,#4243,.T.);
#6022=ORIENTED_EDGE('',*,*,#4244,.F.);
#6023=ORIENTED_EDGE('',*,*,#4245,.T.);
#6024=ORIENTED_EDGE('',*,*,#4241,.T.);
#6025=ORIENTED_EDGE('',*,*,#4246,.T.);
#6026=ORIENTED_EDGE('',*,*,#4247,.F.);
#6027=ORIENTED_EDGE('',*,*,#4248,.T.);
#6028=ORIENTED_EDGE('',*,*,#4244,.T.);
#6029=ORIENTED_EDGE('',*,*,#4249,.T.);
#6030=ORIENTED_EDGE('',*,*,#4250,.F.);
#6031=ORIENTED_EDGE('',*,*,#4251,.T.);
#6032=ORIENTED_EDGE('',*,*,#4247,.T.);
#6033=ORIENTED_EDGE('',*,*,#4252,.T.);
#6034=ORIENTED_EDGE('',*,*,#4253,.F.);
#6035=ORIENTED_EDGE('',*,*,#4254,.T.);
#6036=ORIENTED_EDGE('',*,*,#4250,.T.);
#6037=ORIENTED_EDGE('',*,*,#4255,.T.);
#6038=ORIENTED_EDGE('',*,*,#4256,.F.);
#6039=ORIENTED_EDGE('',*,*,#4257,.T.);
#6040=ORIENTED_EDGE('',*,*,#4253,.T.);
#6041=ORIENTED_EDGE('',*,*,#4258,.T.);
#6042=ORIENTED_EDGE('',*,*,#4259,.F.);
#6043=ORIENTED_EDGE('',*,*,#4260,.T.);
#6044=ORIENTED_EDGE('',*,*,#4256,.T.);
#6045=ORIENTED_EDGE('',*,*,#4261,.T.);
#6046=ORIENTED_EDGE('',*,*,#4262,.F.);
#6047=ORIENTED_EDGE('',*,*,#4263,.T.);
#6048=ORIENTED_EDGE('',*,*,#4259,.T.);
#6049=ORIENTED_EDGE('',*,*,#4264,.T.);
#6050=ORIENTED_EDGE('',*,*,#4265,.F.);
#6051=ORIENTED_EDGE('',*,*,#4266,.T.);
#6052=ORIENTED_EDGE('',*,*,#4262,.T.);
#6053=ORIENTED_EDGE('',*,*,#4267,.T.);
#6054=ORIENTED_EDGE('',*,*,#4268,.F.);
#6055=ORIENTED_EDGE('',*,*,#4269,.T.);
#6056=ORIENTED_EDGE('',*,*,#4265,.T.);
#6057=ORIENTED_EDGE('',*,*,#4270,.T.);
#6058=ORIENTED_EDGE('',*,*,#4271,.F.);
#6059=ORIENTED_EDGE('',*,*,#4272,.T.);
#6060=ORIENTED_EDGE('',*,*,#4268,.T.);
#6061=ORIENTED_EDGE('',*,*,#4273,.T.);
#6062=ORIENTED_EDGE('',*,*,#4274,.F.);
#6063=ORIENTED_EDGE('',*,*,#4275,.T.);
#6064=ORIENTED_EDGE('',*,*,#4271,.T.);
#6065=ORIENTED_EDGE('',*,*,#4276,.T.);
#6066=ORIENTED_EDGE('',*,*,#4277,.F.);
#6067=ORIENTED_EDGE('',*,*,#4278,.T.);
#6068=ORIENTED_EDGE('',*,*,#4274,.T.);
#6069=ORIENTED_EDGE('',*,*,#4279,.T.);
#6070=ORIENTED_EDGE('',*,*,#4280,.F.);
#6071=ORIENTED_EDGE('',*,*,#4281,.T.);
#6072=ORIENTED_EDGE('',*,*,#4277,.T.);
#6073=ORIENTED_EDGE('',*,*,#4282,.T.);
#6074=ORIENTED_EDGE('',*,*,#4283,.F.);
#6075=ORIENTED_EDGE('',*,*,#4284,.T.);
#6076=ORIENTED_EDGE('',*,*,#4280,.T.);
#6077=ORIENTED_EDGE('',*,*,#4285,.T.);
#6078=ORIENTED_EDGE('',*,*,#4286,.F.);
#6079=ORIENTED_EDGE('',*,*,#4287,.T.);
#6080=ORIENTED_EDGE('',*,*,#4283,.T.);
#6081=ORIENTED_EDGE('',*,*,#4288,.T.);
#6082=ORIENTED_EDGE('',*,*,#4289,.F.);
#6083=ORIENTED_EDGE('',*,*,#4290,.T.);
#6084=ORIENTED_EDGE('',*,*,#4286,.T.);
#6085=ORIENTED_EDGE('',*,*,#4291,.T.);
#6086=ORIENTED_EDGE('',*,*,#4292,.F.);
#6087=ORIENTED_EDGE('',*,*,#4293,.T.);
#6088=ORIENTED_EDGE('',*,*,#4289,.T.);
#6089=ORIENTED_EDGE('',*,*,#4294,.T.);
#6090=ORIENTED_EDGE('',*,*,#4295,.F.);
#6091=ORIENTED_EDGE('',*,*,#4296,.T.);
#6092=ORIENTED_EDGE('',*,*,#4292,.T.);
#6093=ORIENTED_EDGE('',*,*,#4297,.T.);
#6094=ORIENTED_EDGE('',*,*,#4298,.F.);
#6095=ORIENTED_EDGE('',*,*,#4299,.T.);
#6096=ORIENTED_EDGE('',*,*,#4295,.T.);
#6097=ORIENTED_EDGE('',*,*,#4300,.T.);
#6098=ORIENTED_EDGE('',*,*,#4301,.F.);
#6099=ORIENTED_EDGE('',*,*,#4302,.T.);
#6100=ORIENTED_EDGE('',*,*,#4298,.T.);
#6101=ORIENTED_EDGE('',*,*,#4303,.T.);
#6102=ORIENTED_EDGE('',*,*,#4304,.F.);
#6103=ORIENTED_EDGE('',*,*,#4305,.T.);
#6104=ORIENTED_EDGE('',*,*,#4301,.T.);
#6105=ORIENTED_EDGE('',*,*,#4306,.T.);
#6106=ORIENTED_EDGE('',*,*,#4307,.F.);
#6107=ORIENTED_EDGE('',*,*,#4308,.T.);
#6108=ORIENTED_EDGE('',*,*,#4304,.T.);
#6109=ORIENTED_EDGE('',*,*,#4309,.T.);
#6110=ORIENTED_EDGE('',*,*,#4310,.F.);
#6111=ORIENTED_EDGE('',*,*,#4311,.T.);
#6112=ORIENTED_EDGE('',*,*,#4307,.T.);
#6113=ORIENTED_EDGE('',*,*,#4312,.T.);
#6114=ORIENTED_EDGE('',*,*,#4313,.F.);
#6115=ORIENTED_EDGE('',*,*,#4314,.T.);
#6116=ORIENTED_EDGE('',*,*,#4315,.T.);
#6117=ORIENTED_EDGE('',*,*,#4316,.F.);
#6118=ORIENTED_EDGE('',*,*,#4317,.F.);
#6119=ORIENTED_EDGE('',*,*,#4318,.T.);
#6120=ORIENTED_EDGE('',*,*,#4313,.T.);
#6121=ORIENTED_EDGE('',*,*,#4319,.F.);
#6122=ORIENTED_EDGE('',*,*,#4320,.F.);
#6123=ORIENTED_EDGE('',*,*,#4321,.T.);
#6124=ORIENTED_EDGE('',*,*,#4317,.T.);
#6125=ORIENTED_EDGE('',*,*,#4322,.F.);
#6126=ORIENTED_EDGE('',*,*,#4323,.F.);
#6127=ORIENTED_EDGE('',*,*,#4324,.T.);
#6128=ORIENTED_EDGE('',*,*,#4320,.T.);
#6129=ORIENTED_EDGE('',*,*,#4325,.F.);
#6130=ORIENTED_EDGE('',*,*,#4326,.F.);
#6131=ORIENTED_EDGE('',*,*,#4327,.T.);
#6132=ORIENTED_EDGE('',*,*,#4323,.T.);
#6133=ORIENTED_EDGE('',*,*,#4328,.F.);
#6134=ORIENTED_EDGE('',*,*,#4329,.F.);
#6135=ORIENTED_EDGE('',*,*,#4330,.T.);
#6136=ORIENTED_EDGE('',*,*,#4326,.T.);
#6137=ORIENTED_EDGE('',*,*,#4331,.F.);
#6138=ORIENTED_EDGE('',*,*,#4332,.F.);
#6139=ORIENTED_EDGE('',*,*,#4333,.T.);
#6140=ORIENTED_EDGE('',*,*,#4329,.T.);
#6141=ORIENTED_EDGE('',*,*,#4334,.F.);
#6142=ORIENTED_EDGE('',*,*,#4335,.F.);
#6143=ORIENTED_EDGE('',*,*,#4336,.T.);
#6144=ORIENTED_EDGE('',*,*,#4332,.T.);
#6145=ORIENTED_EDGE('',*,*,#4337,.F.);
#6146=ORIENTED_EDGE('',*,*,#4338,.F.);
#6147=ORIENTED_EDGE('',*,*,#4339,.T.);
#6148=ORIENTED_EDGE('',*,*,#4335,.T.);
#6149=ORIENTED_EDGE('',*,*,#4340,.F.);
#6150=ORIENTED_EDGE('',*,*,#4341,.F.);
#6151=ORIENTED_EDGE('',*,*,#4342,.T.);
#6152=ORIENTED_EDGE('',*,*,#4338,.T.);
#6153=ORIENTED_EDGE('',*,*,#4343,.F.);
#6154=ORIENTED_EDGE('',*,*,#4344,.F.);
#6155=ORIENTED_EDGE('',*,*,#4345,.T.);
#6156=ORIENTED_EDGE('',*,*,#4341,.T.);
#6157=ORIENTED_EDGE('',*,*,#4346,.F.);
#6158=ORIENTED_EDGE('',*,*,#4347,.F.);
#6159=ORIENTED_EDGE('',*,*,#4348,.T.);
#6160=ORIENTED_EDGE('',*,*,#4344,.T.);
#6161=ORIENTED_EDGE('',*,*,#4349,.F.);
#6162=ORIENTED_EDGE('',*,*,#4350,.F.);
#6163=ORIENTED_EDGE('',*,*,#4351,.T.);
#6164=ORIENTED_EDGE('',*,*,#4347,.T.);
#6165=ORIENTED_EDGE('',*,*,#4352,.F.);
#6166=ORIENTED_EDGE('',*,*,#4353,.F.);
#6167=ORIENTED_EDGE('',*,*,#4354,.T.);
#6168=ORIENTED_EDGE('',*,*,#4350,.T.);
#6169=ORIENTED_EDGE('',*,*,#4355,.F.);
#6170=ORIENTED_EDGE('',*,*,#4356,.F.);
#6171=ORIENTED_EDGE('',*,*,#4357,.T.);
#6172=ORIENTED_EDGE('',*,*,#4353,.T.);
#6173=ORIENTED_EDGE('',*,*,#4358,.F.);
#6174=ORIENTED_EDGE('',*,*,#4359,.F.);
#6175=ORIENTED_EDGE('',*,*,#4360,.T.);
#6176=ORIENTED_EDGE('',*,*,#4356,.T.);
#6177=ORIENTED_EDGE('',*,*,#4361,.F.);
#6178=ORIENTED_EDGE('',*,*,#4362,.F.);
#6179=ORIENTED_EDGE('',*,*,#4363,.T.);
#6180=ORIENTED_EDGE('',*,*,#4359,.T.);
#6181=ORIENTED_EDGE('',*,*,#4364,.F.);
#6182=ORIENTED_EDGE('',*,*,#4365,.F.);
#6183=ORIENTED_EDGE('',*,*,#4366,.T.);
#6184=ORIENTED_EDGE('',*,*,#4362,.T.);
#6185=ORIENTED_EDGE('',*,*,#4367,.F.);
#6186=ORIENTED_EDGE('',*,*,#4368,.F.);
#6187=ORIENTED_EDGE('',*,*,#4369,.T.);
#6188=ORIENTED_EDGE('',*,*,#4365,.T.);
#6189=ORIENTED_EDGE('',*,*,#4370,.F.);
#6190=ORIENTED_EDGE('',*,*,#4371,.F.);
#6191=ORIENTED_EDGE('',*,*,#4372,.T.);
#6192=ORIENTED_EDGE('',*,*,#4368,.T.);
#6193=ORIENTED_EDGE('',*,*,#4373,.F.);
#6194=ORIENTED_EDGE('',*,*,#4374,.F.);
#6195=ORIENTED_EDGE('',*,*,#4375,.T.);
#6196=ORIENTED_EDGE('',*,*,#4371,.T.);
#6197=ORIENTED_EDGE('',*,*,#4376,.F.);
#6198=ORIENTED_EDGE('',*,*,#4377,.F.);
#6199=ORIENTED_EDGE('',*,*,#4378,.T.);
#6200=ORIENTED_EDGE('',*,*,#4374,.T.);
#6201=ORIENTED_EDGE('',*,*,#4379,.F.);
#6202=ORIENTED_EDGE('',*,*,#4380,.F.);
#6203=ORIENTED_EDGE('',*,*,#4381,.T.);
#6204=ORIENTED_EDGE('',*,*,#4377,.T.);
#6205=ORIENTED_EDGE('',*,*,#4382,.F.);
#6206=ORIENTED_EDGE('',*,*,#4383,.F.);
#6207=ORIENTED_EDGE('',*,*,#4384,.T.);
#6208=ORIENTED_EDGE('',*,*,#4380,.T.);
#6209=ORIENTED_EDGE('',*,*,#4385,.F.);
#6210=ORIENTED_EDGE('',*,*,#4386,.F.);
#6211=ORIENTED_EDGE('',*,*,#4387,.T.);
#6212=ORIENTED_EDGE('',*,*,#4383,.T.);
#6213=ORIENTED_EDGE('',*,*,#4388,.F.);
#6214=ORIENTED_EDGE('',*,*,#4389,.F.);
#6215=ORIENTED_EDGE('',*,*,#4390,.T.);
#6216=ORIENTED_EDGE('',*,*,#4386,.T.);
#6217=ORIENTED_EDGE('',*,*,#4391,.F.);
#6218=ORIENTED_EDGE('',*,*,#4392,.F.);
#6219=ORIENTED_EDGE('',*,*,#4393,.T.);
#6220=ORIENTED_EDGE('',*,*,#4389,.T.);
#6221=ORIENTED_EDGE('',*,*,#4394,.F.);
#6222=ORIENTED_EDGE('',*,*,#4395,.F.);
#6223=ORIENTED_EDGE('',*,*,#4396,.T.);
#6224=ORIENTED_EDGE('',*,*,#4392,.T.);
#6225=ORIENTED_EDGE('',*,*,#4397,.F.);
#6226=ORIENTED_EDGE('',*,*,#4398,.F.);
#6227=ORIENTED_EDGE('',*,*,#4399,.T.);
#6228=ORIENTED_EDGE('',*,*,#4395,.T.);
#6229=ORIENTED_EDGE('',*,*,#4400,.F.);
#6230=ORIENTED_EDGE('',*,*,#4401,.F.);
#6231=ORIENTED_EDGE('',*,*,#4402,.T.);
#6232=ORIENTED_EDGE('',*,*,#4398,.T.);
#6233=ORIENTED_EDGE('',*,*,#4403,.F.);
#6234=ORIENTED_EDGE('',*,*,#4404,.F.);
#6235=ORIENTED_EDGE('',*,*,#4315,.F.);
#6236=ORIENTED_EDGE('',*,*,#4405,.F.);
#6237=ORIENTED_EDGE('',*,*,#4406,.F.);
#6238=ORIENTED_EDGE('',*,*,#4407,.F.);
#6239=ORIENTED_EDGE('',*,*,#4408,.T.);
#6240=ORIENTED_EDGE('',*,*,#4409,.F.);
#6241=ORIENTED_EDGE('',*,*,#4408,.F.);
#6242=ORIENTED_EDGE('',*,*,#4405,.T.);
#6243=ORIENTED_EDGE('',*,*,#4314,.F.);
#6244=ORIENTED_EDGE('',*,*,#4318,.F.);
#6245=ORIENTED_EDGE('',*,*,#4321,.F.);
#6246=ORIENTED_EDGE('',*,*,#4324,.F.);
#6247=ORIENTED_EDGE('',*,*,#4327,.F.);
#6248=ORIENTED_EDGE('',*,*,#4330,.F.);
#6249=ORIENTED_EDGE('',*,*,#4333,.F.);
#6250=ORIENTED_EDGE('',*,*,#4336,.F.);
#6251=ORIENTED_EDGE('',*,*,#4339,.F.);
#6252=ORIENTED_EDGE('',*,*,#4342,.F.);
#6253=ORIENTED_EDGE('',*,*,#4345,.F.);
#6254=ORIENTED_EDGE('',*,*,#4348,.F.);
#6255=ORIENTED_EDGE('',*,*,#4351,.F.);
#6256=ORIENTED_EDGE('',*,*,#4354,.F.);
#6257=ORIENTED_EDGE('',*,*,#4357,.F.);
#6258=ORIENTED_EDGE('',*,*,#4360,.F.);
#6259=ORIENTED_EDGE('',*,*,#4363,.F.);
#6260=ORIENTED_EDGE('',*,*,#4366,.F.);
#6261=ORIENTED_EDGE('',*,*,#4369,.F.);
#6262=ORIENTED_EDGE('',*,*,#4372,.F.);
#6263=ORIENTED_EDGE('',*,*,#4375,.F.);
#6264=ORIENTED_EDGE('',*,*,#4378,.F.);
#6265=ORIENTED_EDGE('',*,*,#4381,.F.);
#6266=ORIENTED_EDGE('',*,*,#4384,.F.);
#6267=ORIENTED_EDGE('',*,*,#4387,.F.);
#6268=ORIENTED_EDGE('',*,*,#4390,.F.);
#6269=ORIENTED_EDGE('',*,*,#4393,.F.);
#6270=ORIENTED_EDGE('',*,*,#4396,.F.);
#6271=ORIENTED_EDGE('',*,*,#4399,.F.);
#6272=ORIENTED_EDGE('',*,*,#4402,.F.);
#6273=ORIENTED_EDGE('',*,*,#4410,.F.);
#6274=ORIENTED_EDGE('',*,*,#4411,.F.);
#6275=ORIENTED_EDGE('',*,*,#4223,.F.);
#6276=ORIENTED_EDGE('',*,*,#4227,.F.);
#6277=ORIENTED_EDGE('',*,*,#4230,.F.);
#6278=ORIENTED_EDGE('',*,*,#4233,.F.);
#6279=ORIENTED_EDGE('',*,*,#4236,.F.);
#6280=ORIENTED_EDGE('',*,*,#4239,.F.);
#6281=ORIENTED_EDGE('',*,*,#4242,.F.);
#6282=ORIENTED_EDGE('',*,*,#4245,.F.);
#6283=ORIENTED_EDGE('',*,*,#4248,.F.);
#6284=ORIENTED_EDGE('',*,*,#4251,.F.);
#6285=ORIENTED_EDGE('',*,*,#4254,.F.);
#6286=ORIENTED_EDGE('',*,*,#4257,.F.);
#6287=ORIENTED_EDGE('',*,*,#4260,.F.);
#6288=ORIENTED_EDGE('',*,*,#4263,.F.);
#6289=ORIENTED_EDGE('',*,*,#4266,.F.);
#6290=ORIENTED_EDGE('',*,*,#4269,.F.);
#6291=ORIENTED_EDGE('',*,*,#4272,.F.);
#6292=ORIENTED_EDGE('',*,*,#4275,.F.);
#6293=ORIENTED_EDGE('',*,*,#4278,.F.);
#6294=ORIENTED_EDGE('',*,*,#4281,.F.);
#6295=ORIENTED_EDGE('',*,*,#4284,.F.);
#6296=ORIENTED_EDGE('',*,*,#4287,.F.);
#6297=ORIENTED_EDGE('',*,*,#4290,.F.);
#6298=ORIENTED_EDGE('',*,*,#4293,.F.);
#6299=ORIENTED_EDGE('',*,*,#4296,.F.);
#6300=ORIENTED_EDGE('',*,*,#4299,.F.);
#6301=ORIENTED_EDGE('',*,*,#4302,.F.);
#6302=ORIENTED_EDGE('',*,*,#4305,.F.);
#6303=ORIENTED_EDGE('',*,*,#4308,.F.);
#6304=ORIENTED_EDGE('',*,*,#4311,.F.);
#6305=ORIENTED_EDGE('',*,*,#4412,.F.);
#6306=ORIENTED_EDGE('',*,*,#4401,.T.);
#6307=ORIENTED_EDGE('',*,*,#4413,.F.);
#6308=ORIENTED_EDGE('',*,*,#4414,.F.);
#6309=ORIENTED_EDGE('',*,*,#4410,.T.);
#6310=ORIENTED_EDGE('',*,*,#4404,.T.);
#6311=ORIENTED_EDGE('',*,*,#4407,.T.);
#6312=ORIENTED_EDGE('',*,*,#4415,.F.);
#6313=ORIENTED_EDGE('',*,*,#4312,.F.);
#6314=ORIENTED_EDGE('',*,*,#4309,.F.);
#6315=ORIENTED_EDGE('',*,*,#4306,.F.);
#6316=ORIENTED_EDGE('',*,*,#4303,.F.);
#6317=ORIENTED_EDGE('',*,*,#4300,.F.);
#6318=ORIENTED_EDGE('',*,*,#4297,.F.);
#6319=ORIENTED_EDGE('',*,*,#4294,.F.);
#6320=ORIENTED_EDGE('',*,*,#4291,.F.);
#6321=ORIENTED_EDGE('',*,*,#4288,.F.);
#6322=ORIENTED_EDGE('',*,*,#4285,.F.);
#6323=ORIENTED_EDGE('',*,*,#4282,.F.);
#6324=ORIENTED_EDGE('',*,*,#4279,.F.);
#6325=ORIENTED_EDGE('',*,*,#4276,.F.);
#6326=ORIENTED_EDGE('',*,*,#4273,.F.);
#6327=ORIENTED_EDGE('',*,*,#4270,.F.);
#6328=ORIENTED_EDGE('',*,*,#4267,.F.);
#6329=ORIENTED_EDGE('',*,*,#4264,.F.);
#6330=ORIENTED_EDGE('',*,*,#4261,.F.);
#6331=ORIENTED_EDGE('',*,*,#4258,.F.);
#6332=ORIENTED_EDGE('',*,*,#4255,.F.);
#6333=ORIENTED_EDGE('',*,*,#4252,.F.);
#6334=ORIENTED_EDGE('',*,*,#4249,.F.);
#6335=ORIENTED_EDGE('',*,*,#4246,.F.);
#6336=ORIENTED_EDGE('',*,*,#4243,.F.);
#6337=ORIENTED_EDGE('',*,*,#4240,.F.);
#6338=ORIENTED_EDGE('',*,*,#4237,.F.);
#6339=ORIENTED_EDGE('',*,*,#4234,.F.);
#6340=ORIENTED_EDGE('',*,*,#4231,.F.);
#6341=ORIENTED_EDGE('',*,*,#4228,.F.);
#6342=ORIENTED_EDGE('',*,*,#4225,.F.);
#6343=ORIENTED_EDGE('',*,*,#4416,.F.);
#6344=ORIENTED_EDGE('',*,*,#4413,.T.);
#6345=ORIENTED_EDGE('',*,*,#4403,.T.);
#6346=ORIENTED_EDGE('',*,*,#4400,.T.);
#6347=ORIENTED_EDGE('',*,*,#4397,.T.);
#6348=ORIENTED_EDGE('',*,*,#4394,.T.);
#6349=ORIENTED_EDGE('',*,*,#4391,.T.);
#6350=ORIENTED_EDGE('',*,*,#4388,.T.);
#6351=ORIENTED_EDGE('',*,*,#4385,.T.);
#6352=ORIENTED_EDGE('',*,*,#4382,.T.);
#6353=ORIENTED_EDGE('',*,*,#4379,.T.);
#6354=ORIENTED_EDGE('',*,*,#4376,.T.);
#6355=ORIENTED_EDGE('',*,*,#4373,.T.);
#6356=ORIENTED_EDGE('',*,*,#4370,.T.);
#6357=ORIENTED_EDGE('',*,*,#4367,.T.);
#6358=ORIENTED_EDGE('',*,*,#4364,.T.);
#6359=ORIENTED_EDGE('',*,*,#4361,.T.);
#6360=ORIENTED_EDGE('',*,*,#4358,.T.);
#6361=ORIENTED_EDGE('',*,*,#4355,.T.);
#6362=ORIENTED_EDGE('',*,*,#4352,.T.);
#6363=ORIENTED_EDGE('',*,*,#4349,.T.);
#6364=ORIENTED_EDGE('',*,*,#4346,.T.);
#6365=ORIENTED_EDGE('',*,*,#4343,.T.);
#6366=ORIENTED_EDGE('',*,*,#4340,.T.);
#6367=ORIENTED_EDGE('',*,*,#4337,.T.);
#6368=ORIENTED_EDGE('',*,*,#4334,.T.);
#6369=ORIENTED_EDGE('',*,*,#4331,.T.);
#6370=ORIENTED_EDGE('',*,*,#4328,.T.);
#6371=ORIENTED_EDGE('',*,*,#4325,.T.);
#6372=ORIENTED_EDGE('',*,*,#4322,.T.);
#6373=ORIENTED_EDGE('',*,*,#4319,.T.);
#6374=ORIENTED_EDGE('',*,*,#4316,.T.);
#6375=ORIENTED_EDGE('',*,*,#4310,.T.);
#6376=ORIENTED_EDGE('',*,*,#4415,.T.);
#6377=ORIENTED_EDGE('',*,*,#4406,.T.);
#6378=ORIENTED_EDGE('',*,*,#4412,.T.);
#6379=ORIENTED_EDGE('',*,*,#4417,.F.);
#6380=ORIENTED_EDGE('',*,*,#4418,.T.);
#6381=ORIENTED_EDGE('',*,*,#4419,.T.);
#6382=ORIENTED_EDGE('',*,*,#4420,.F.);
#6383=ORIENTED_EDGE('',*,*,#4421,.F.);
#6384=ORIENTED_EDGE('',*,*,#4422,.T.);
#6385=ORIENTED_EDGE('',*,*,#4423,.T.);
#6386=ORIENTED_EDGE('',*,*,#4418,.F.);
#6387=ORIENTED_EDGE('',*,*,#4424,.F.);
#6388=ORIENTED_EDGE('',*,*,#4425,.T.);
#6389=ORIENTED_EDGE('',*,*,#4426,.T.);
#6390=ORIENTED_EDGE('',*,*,#4422,.F.);
#6391=ORIENTED_EDGE('',*,*,#4427,.F.);
#6392=ORIENTED_EDGE('',*,*,#4428,.T.);
#6393=ORIENTED_EDGE('',*,*,#4429,.T.);
#6394=ORIENTED_EDGE('',*,*,#4425,.F.);
#6395=ORIENTED_EDGE('',*,*,#4430,.F.);
#6396=ORIENTED_EDGE('',*,*,#4431,.T.);
#6397=ORIENTED_EDGE('',*,*,#4432,.T.);
#6398=ORIENTED_EDGE('',*,*,#4428,.F.);
#6399=ORIENTED_EDGE('',*,*,#4433,.F.);
#6400=ORIENTED_EDGE('',*,*,#4420,.T.);
#6401=ORIENTED_EDGE('',*,*,#4434,.T.);
#6402=ORIENTED_EDGE('',*,*,#4431,.F.);
#6403=ORIENTED_EDGE('',*,*,#4434,.F.);
#6404=ORIENTED_EDGE('',*,*,#4419,.F.);
#6405=ORIENTED_EDGE('',*,*,#4423,.F.);
#6406=ORIENTED_EDGE('',*,*,#4426,.F.);
#6407=ORIENTED_EDGE('',*,*,#4429,.F.);
#6408=ORIENTED_EDGE('',*,*,#4432,.F.);
#6409=ORIENTED_EDGE('',*,*,#4435,.T.);
#6410=ORIENTED_EDGE('',*,*,#4411,.T.);
#6411=ORIENTED_EDGE('',*,*,#4414,.T.);
#6412=ORIENTED_EDGE('',*,*,#4416,.T.);
#6413=ORIENTED_EDGE('',*,*,#4224,.F.);
#6414=ORIENTED_EDGE('',*,*,#4435,.F.);
#6415=ORIENTED_EDGE('',*,*,#4436,.T.);
#6416=ORIENTED_EDGE('',*,*,#4437,.T.);
#6417=ORIENTED_EDGE('',*,*,#4436,.F.);
#6418=ORIENTED_EDGE('',*,*,#4437,.F.);
#6419=ORIENTED_EDGE('',*,*,#4417,.T.);
#6420=ORIENTED_EDGE('',*,*,#4433,.T.);
#6421=ORIENTED_EDGE('',*,*,#4430,.T.);
#6422=ORIENTED_EDGE('',*,*,#4427,.T.);
#6423=ORIENTED_EDGE('',*,*,#4424,.T.);
#6424=ORIENTED_EDGE('',*,*,#4421,.T.);
#6425=ORIENTED_EDGE('',*,*,#4409,.T.);
#6426=ORIENTED_EDGE('',*,*,#4438,.T.);
#6427=ORIENTED_EDGE('',*,*,#4439,.F.);
#6428=ORIENTED_EDGE('',*,*,#4440,.T.);
#6429=ORIENTED_EDGE('',*,*,#4441,.T.);
#6430=ORIENTED_EDGE('',*,*,#4442,.T.);
#6431=ORIENTED_EDGE('',*,*,#4443,.F.);
#6432=ORIENTED_EDGE('',*,*,#4438,.F.);
#6433=ORIENTED_EDGE('',*,*,#4444,.T.);
#6434=ORIENTED_EDGE('',*,*,#4445,.T.);
#6435=ORIENTED_EDGE('',*,*,#4446,.T.);
#6436=ORIENTED_EDGE('',*,*,#4441,.F.);
#6437=ORIENTED_EDGE('',*,*,#4447,.T.);
#6438=ORIENTED_EDGE('',*,*,#4448,.T.);
#6439=ORIENTED_EDGE('',*,*,#4449,.T.);
#6440=ORIENTED_EDGE('',*,*,#4445,.F.);
#6441=ORIENTED_EDGE('',*,*,#4450,.T.);
#6442=ORIENTED_EDGE('',*,*,#4451,.F.);
#6443=ORIENTED_EDGE('',*,*,#4452,.T.);
#6444=ORIENTED_EDGE('',*,*,#4453,.F.);
#6445=ORIENTED_EDGE('',*,*,#4454,.T.);
#6446=ORIENTED_EDGE('',*,*,#4455,.T.);
#6447=ORIENTED_EDGE('',*,*,#4456,.T.);
#6448=ORIENTED_EDGE('',*,*,#4457,.F.);
#6449=ORIENTED_EDGE('',*,*,#4458,.F.);
#6450=ORIENTED_EDGE('',*,*,#4459,.T.);
#6451=ORIENTED_EDGE('',*,*,#4460,.T.);
#6452=ORIENTED_EDGE('',*,*,#4455,.F.);
#6453=ORIENTED_EDGE('',*,*,#4461,.F.);
#6454=ORIENTED_EDGE('',*,*,#4462,.T.);
#6455=ORIENTED_EDGE('',*,*,#4463,.T.);
#6456=ORIENTED_EDGE('',*,*,#4459,.F.);
#6457=ORIENTED_EDGE('',*,*,#4464,.F.);
#6458=ORIENTED_EDGE('',*,*,#4465,.T.);
#6459=ORIENTED_EDGE('',*,*,#4466,.T.);
#6460=ORIENTED_EDGE('',*,*,#4462,.F.);
#6461=ORIENTED_EDGE('',*,*,#4467,.F.);
#6462=ORIENTED_EDGE('',*,*,#4468,.F.);
#6463=ORIENTED_EDGE('',*,*,#4469,.F.);
#6464=ORIENTED_EDGE('',*,*,#4470,.F.);
#6465=ORIENTED_EDGE('',*,*,#4471,.T.);
#6466=ORIENTED_EDGE('',*,*,#4468,.T.);
#6467=ORIENTED_EDGE('',*,*,#4472,.T.);
#6468=ORIENTED_EDGE('',*,*,#4465,.F.);
#6469=ORIENTED_EDGE('',*,*,#4473,.F.);
#6470=ORIENTED_EDGE('',*,*,#4474,.F.);
#6471=ORIENTED_EDGE('',*,*,#4456,.F.);
#6472=ORIENTED_EDGE('',*,*,#4460,.F.);
#6473=ORIENTED_EDGE('',*,*,#4463,.F.);
#6474=ORIENTED_EDGE('',*,*,#4466,.F.);
#6475=ORIENTED_EDGE('',*,*,#4472,.F.);
#6476=ORIENTED_EDGE('',*,*,#4471,.F.);
#6477=ORIENTED_EDGE('',*,*,#4475,.F.);
#6478=ORIENTED_EDGE('',*,*,#4452,.F.);
#6479=ORIENTED_EDGE('',*,*,#4476,.F.);
#6480=ORIENTED_EDGE('',*,*,#4450,.F.);
#6481=ORIENTED_EDGE('',*,*,#4447,.F.);
#6482=ORIENTED_EDGE('',*,*,#4444,.F.);
#6483=ORIENTED_EDGE('',*,*,#4440,.F.);
#6484=ORIENTED_EDGE('',*,*,#4477,.F.);
#6485=ORIENTED_EDGE('',*,*,#4442,.F.);
#6486=ORIENTED_EDGE('',*,*,#4446,.F.);
#6487=ORIENTED_EDGE('',*,*,#4449,.F.);
#6488=ORIENTED_EDGE('',*,*,#4478,.F.);
#6489=ORIENTED_EDGE('',*,*,#4454,.F.);
#6490=ORIENTED_EDGE('',*,*,#4479,.F.);
#6491=ORIENTED_EDGE('',*,*,#4469,.T.);
#6492=ORIENTED_EDGE('',*,*,#4473,.T.);
#6493=ORIENTED_EDGE('',*,*,#4467,.T.);
#6494=ORIENTED_EDGE('',*,*,#4464,.T.);
#6495=ORIENTED_EDGE('',*,*,#4461,.T.);
#6496=ORIENTED_EDGE('',*,*,#4458,.T.);
#6497=ORIENTED_EDGE('',*,*,#4480,.T.);
#6498=ORIENTED_EDGE('',*,*,#4481,.T.);
#6499=ORIENTED_EDGE('',*,*,#4482,.T.);
#6500=ORIENTED_EDGE('',*,*,#4483,.T.);
#6501=ORIENTED_EDGE('',*,*,#4484,.T.);
#6502=ORIENTED_EDGE('',*,*,#4485,.T.);
#6503=ORIENTED_EDGE('',*,*,#4475,.T.);
#6504=ORIENTED_EDGE('',*,*,#4470,.T.);
#6505=ORIENTED_EDGE('',*,*,#4479,.T.);
#6506=ORIENTED_EDGE('',*,*,#4453,.T.);
#6507=ORIENTED_EDGE('',*,*,#4451,.T.);
#6508=ORIENTED_EDGE('',*,*,#4478,.T.);
#6509=ORIENTED_EDGE('',*,*,#4448,.F.);
#6510=ORIENTED_EDGE('',*,*,#4476,.T.);
#6511=ORIENTED_EDGE('',*,*,#4486,.T.);
#6512=ORIENTED_EDGE('',*,*,#4487,.T.);
#6513=ORIENTED_EDGE('',*,*,#4485,.F.);
#6514=ORIENTED_EDGE('',*,*,#4488,.F.);
#6515=ORIENTED_EDGE('',*,*,#4489,.T.);
#6516=ORIENTED_EDGE('',*,*,#4488,.T.);
#6517=ORIENTED_EDGE('',*,*,#4484,.F.);
#6518=ORIENTED_EDGE('',*,*,#4490,.F.);
#6519=ORIENTED_EDGE('',*,*,#4491,.T.);
#6520=ORIENTED_EDGE('',*,*,#4490,.T.);
#6521=ORIENTED_EDGE('',*,*,#4483,.F.);
#6522=ORIENTED_EDGE('',*,*,#4492,.F.);
#6523=ORIENTED_EDGE('',*,*,#4493,.T.);
#6524=ORIENTED_EDGE('',*,*,#4492,.T.);
#6525=ORIENTED_EDGE('',*,*,#4482,.F.);
#6526=ORIENTED_EDGE('',*,*,#4494,.F.);
#6527=ORIENTED_EDGE('',*,*,#4495,.T.);
#6528=ORIENTED_EDGE('',*,*,#4494,.T.);
#6529=ORIENTED_EDGE('',*,*,#4481,.F.);
#6530=ORIENTED_EDGE('',*,*,#4496,.F.);
#6531=ORIENTED_EDGE('',*,*,#4497,.T.);
#6532=ORIENTED_EDGE('',*,*,#4496,.T.);
#6533=ORIENTED_EDGE('',*,*,#4480,.F.);
#6534=ORIENTED_EDGE('',*,*,#4487,.F.);
#6535=ORIENTED_EDGE('',*,*,#4497,.F.);
#6536=ORIENTED_EDGE('',*,*,#4486,.F.);
#6537=ORIENTED_EDGE('',*,*,#4489,.F.);
#6538=ORIENTED_EDGE('',*,*,#4491,.F.);
#6539=ORIENTED_EDGE('',*,*,#4493,.F.);
#6540=ORIENTED_EDGE('',*,*,#4495,.F.);
#6541=ORIENTED_EDGE('',*,*,#4474,.T.);
#6542=ORIENTED_EDGE('',*,*,#4439,.T.);
#6543=ORIENTED_EDGE('',*,*,#4443,.T.);
#6544=ORIENTED_EDGE('',*,*,#4477,.T.);
#6545=ORIENTED_EDGE('',*,*,#4457,.T.);
#6546=ORIENTED_EDGE('',*,*,#4498,.F.);
#6547=ORIENTED_EDGE('',*,*,#4499,.T.);
#6548=ORIENTED_EDGE('',*,*,#4500,.T.);
#6549=ORIENTED_EDGE('',*,*,#4499,.F.);
#6550=ORIENTED_EDGE('',*,*,#4501,.F.);
#6551=ORIENTED_EDGE('',*,*,#4502,.T.);
#6552=ORIENTED_EDGE('',*,*,#4503,.T.);
#6553=ORIENTED_EDGE('',*,*,#4502,.F.);
#6554=ORIENTED_EDGE('',*,*,#4501,.T.);
#6555=ORIENTED_EDGE('',*,*,#4498,.T.);
#6556=ORIENTED_EDGE('',*,*,#4503,.F.);
#6557=ORIENTED_EDGE('',*,*,#4500,.F.);
#6558=CYLINDRICAL_SURFACE('',#7226,0.17);
#6559=CYLINDRICAL_SURFACE('',#7229,0.17);
#6560=CYLINDRICAL_SURFACE('',#7232,0.41);
#6561=CYLINDRICAL_SURFACE('',#7242,0.2);
#6562=CYLINDRICAL_SURFACE('',#7245,6.99668559332711);
#6563=CYLINDRICAL_SURFACE('',#7253,1.4);
#6564=CYLINDRICAL_SURFACE('',#7256,1.4);
#6565=CYLINDRICAL_SURFACE('',#7267,1.1);
#6566=CYLINDRICAL_SURFACE('',#7275,1.7);
#6567=CYLINDRICAL_SURFACE('',#7276,1.7);
#6568=CYLINDRICAL_SURFACE('',#7286,0.17);
#6569=CYLINDRICAL_SURFACE('',#7289,0.17);
#6570=CYLINDRICAL_SURFACE('',#7292,0.41);
#6571=CYLINDRICAL_SURFACE('',#7297,2.9940843367589);
#6572=CYLINDRICAL_SURFACE('',#7300,0.3);
#6573=CYLINDRICAL_SURFACE('',#7303,7.11398555645532);
#6574=CYLINDRICAL_SURFACE('',#7311,1.4);
#6575=CYLINDRICAL_SURFACE('',#7314,1.4);
#6576=CYLINDRICAL_SURFACE('',#7325,1.1);
#6577=CYLINDRICAL_SURFACE('',#7333,1.7);
#6578=CYLINDRICAL_SURFACE('',#7334,1.7);
#6579=CYLINDRICAL_SURFACE('',#7344,0.3);
#6580=CYLINDRICAL_SURFACE('',#7351,0.4);
#6581=CYLINDRICAL_SURFACE('',#7356,0.6);
#6582=CYLINDRICAL_SURFACE('',#7359,0.4);
#6583=CYLINDRICAL_SURFACE('',#7367,0.3);
#6584=CYLINDRICAL_SURFACE('',#7369,0.6);
#6585=CYLINDRICAL_SURFACE('',#7378,0.15);
#6586=CYLINDRICAL_SURFACE('',#7381,0.15);
#6587=CYLINDRICAL_SURFACE('',#7383,0.15);
#6588=CYLINDRICAL_SURFACE('',#7385,0.15);
#6589=CYLINDRICAL_SURFACE('',#7388,0.3);
#6590=CYLINDRICAL_SURFACE('',#7393,0.3);
#6591=CYLINDRICAL_SURFACE('',#7398,0.17);
#6592=CYLINDRICAL_SURFACE('',#7400,0.17);
#6593=CYLINDRICAL_SURFACE('',#7424,0.4);
#6594=CYLINDRICAL_SURFACE('',#7426,0.4);
#6595=CYLINDRICAL_SURFACE('',#7448,0.1);
#6596=CYLINDRICAL_SURFACE('',#7452,0.1);
#6597=CYLINDRICAL_SURFACE('',#7466,0.3);
#6598=CYLINDRICAL_SURFACE('',#7471,0.3);
#6599=CYLINDRICAL_SURFACE('',#7480,0.15);
#6600=CYLINDRICAL_SURFACE('',#7483,0.15);
#6601=CYLINDRICAL_SURFACE('',#7485,0.15);
#6602=CYLINDRICAL_SURFACE('',#7487,0.15);
#6603=CYLINDRICAL_SURFACE('',#7506,0.17);
#6604=CYLINDRICAL_SURFACE('',#7508,0.17);
#6605=CYLINDRICAL_SURFACE('',#7532,0.4);
#6606=CYLINDRICAL_SURFACE('',#7534,0.4);
#6607=CYLINDRICAL_SURFACE('',#7556,0.1);
#6608=CYLINDRICAL_SURFACE('',#7560,0.1);
#6609=CYLINDRICAL_SURFACE('',#7574,0.3);
#6610=CYLINDRICAL_SURFACE('',#7579,0.3);
#6611=CYLINDRICAL_SURFACE('',#7584,0.35);
#6612=CYLINDRICAL_SURFACE('',#7587,0.35);
#6613=CYLINDRICAL_SURFACE('',#7593,0.25);
#6614=CYLINDRICAL_SURFACE('',#7599,0.25);
#6615=CYLINDRICAL_SURFACE('',#7605,0.25);
#6616=CYLINDRICAL_SURFACE('',#7611,0.25);
#6617=CYLINDRICAL_SURFACE('',#7614,0.15);
#6618=CYLINDRICAL_SURFACE('',#7616,0.15);
#6619=CYLINDRICAL_SURFACE('',#7618,0.15);
#6620=CYLINDRICAL_SURFACE('',#7620,0.15);
#6621=CYLINDRICAL_SURFACE('',#7624,0.08);
#6622=CYLINDRICAL_SURFACE('',#7629,0.08);
#6623=CYLINDRICAL_SURFACE('',#7637,0.14635);
#6624=CYLINDRICAL_SURFACE('',#7639,0.14635);
#6625=CYLINDRICAL_SURFACE('',#7640,0.14635);
#6626=CYLINDRICAL_SURFACE('',#7641,0.14635);
#6627=CYLINDRICAL_SURFACE('',#7642,0.14635);
#6628=CYLINDRICAL_SURFACE('',#7643,0.14635);
#6629=CYLINDRICAL_SURFACE('',#7644,0.14635);
#6630=CYLINDRICAL_SURFACE('',#7645,0.14635);
#6631=CYLINDRICAL_SURFACE('',#7646,0.14635);
#6632=CYLINDRICAL_SURFACE('',#7647,0.14635);
#6633=CYLINDRICAL_SURFACE('',#7648,0.14635);
#6634=CYLINDRICAL_SURFACE('',#7649,0.14635);
#6635=CYLINDRICAL_SURFACE('',#7650,0.14635);
#6636=CYLINDRICAL_SURFACE('',#7651,0.14635);
#6637=CYLINDRICAL_SURFACE('',#7652,0.14635);
#6638=CYLINDRICAL_SURFACE('',#7653,0.14635);
#6639=CYLINDRICAL_SURFACE('',#7654,0.14635);
#6640=CYLINDRICAL_SURFACE('',#7655,0.14635);
#6641=CYLINDRICAL_SURFACE('',#7656,0.14635);
#6642=CYLINDRICAL_SURFACE('',#7657,0.14635);
#6643=CYLINDRICAL_SURFACE('',#7658,0.14635);
#6644=CYLINDRICAL_SURFACE('',#7659,0.14635);
#6645=CYLINDRICAL_SURFACE('',#7660,0.14635);
#6646=CYLINDRICAL_SURFACE('',#7661,0.14635);
#6647=CYLINDRICAL_SURFACE('',#7662,0.14635);
#6648=CYLINDRICAL_SURFACE('',#7663,0.14635);
#6649=CYLINDRICAL_SURFACE('',#7664,0.14635);
#6650=CYLINDRICAL_SURFACE('',#7665,0.14635);
#6651=CYLINDRICAL_SURFACE('',#7666,0.14635);
#6652=CYLINDRICAL_SURFACE('',#7667,0.14635);
#6653=CYLINDRICAL_SURFACE('',#7668,0.117775);
#6654=CYLINDRICAL_SURFACE('',#7670,0.117775);
#6655=CYLINDRICAL_SURFACE('',#7671,0.117775);
#6656=CYLINDRICAL_SURFACE('',#7672,0.117775);
#6657=CYLINDRICAL_SURFACE('',#7673,0.117775);
#6658=CYLINDRICAL_SURFACE('',#7674,0.117775);
#6659=CYLINDRICAL_SURFACE('',#7675,0.117775);
#6660=CYLINDRICAL_SURFACE('',#7676,0.117775);
#6661=CYLINDRICAL_SURFACE('',#7677,0.117775);
#6662=CYLINDRICAL_SURFACE('',#7678,0.117775);
#6663=CYLINDRICAL_SURFACE('',#7679,0.117775);
#6664=CYLINDRICAL_SURFACE('',#7680,0.117775);
#6665=CYLINDRICAL_SURFACE('',#7681,0.117775);
#6666=CYLINDRICAL_SURFACE('',#7682,0.117775);
#6667=CYLINDRICAL_SURFACE('',#7683,0.117775);
#6668=CYLINDRICAL_SURFACE('',#7684,0.117775);
#6669=CYLINDRICAL_SURFACE('',#7685,0.117775);
#6670=CYLINDRICAL_SURFACE('',#7686,0.117775);
#6671=CYLINDRICAL_SURFACE('',#7687,0.117775);
#6672=CYLINDRICAL_SURFACE('',#7688,0.117775);
#6673=CYLINDRICAL_SURFACE('',#7689,0.117775);
#6674=CYLINDRICAL_SURFACE('',#7690,0.117775);
#6675=CYLINDRICAL_SURFACE('',#7691,0.117775);
#6676=CYLINDRICAL_SURFACE('',#7692,0.117775);
#6677=CYLINDRICAL_SURFACE('',#7693,0.117775);
#6678=CYLINDRICAL_SURFACE('',#7694,0.117775);
#6679=CYLINDRICAL_SURFACE('',#7695,0.117775);
#6680=CYLINDRICAL_SURFACE('',#7696,0.117775);
#6681=CYLINDRICAL_SURFACE('',#7697,0.117775);
#6682=CYLINDRICAL_SURFACE('',#7698,0.117775);
#6683=CYLINDRICAL_SURFACE('',#7702,0.117775);
#6684=CYLINDRICAL_SURFACE('',#7704,0.14635);
#6685=CYLINDRICAL_SURFACE('',#7714,0.275);
#6686=CYLINDRICAL_SURFACE('',#7719,0.12645);
#6687=CYLINDRICAL_SURFACE('',#7721,0.12645);
#6688=CYLINDRICAL_SURFACE('',#7723,0.12645);
#6689=CYLINDRICAL_SURFACE('',#7724,0.12645);
#6690=CYLINDRICAL_SURFACE('',#7725,0.12645);
#6691=CYLINDRICAL_SURFACE('',#7727,0.1543);
#6692=CYLINDRICAL_SURFACE('',#7729,0.1543);
#6693=CYLINDRICAL_SURFACE('',#7730,0.1543);
#6694=CYLINDRICAL_SURFACE('',#7731,0.1543);
#6695=CYLINDRICAL_SURFACE('',#7732,0.1543);
#6696=CYLINDRICAL_SURFACE('',#7734,0.1543);
#6697=CYLINDRICAL_SURFACE('',#7736,0.12645);
#6698=CYLINDRICAL_SURFACE('',#7753,0.41);
#6699=CYLINDRICAL_SURFACE('',#7756,0.6);
#6700=ADVANCED_FACE('',(#821),#6558,.F.);
#6701=ADVANCED_FACE('',(#822),#6559,.F.);
#6702=ADVANCED_FACE('',(#823),#6560,.F.);
#6703=ADVANCED_FACE('',(#824),#662,.F.);
#6704=ADVANCED_FACE('',(#825),#660,.T.);
#6705=ADVANCED_FACE('',(#826),#663,.T.);
#6706=ADVANCED_FACE('',(#827),#664,.T.);
#6707=ADVANCED_FACE('',(#828),#665,.T.);
#6708=ADVANCED_FACE('',(#829),#6561,.T.);
#6709=ADVANCED_FACE('',(#830),#6562,.T.);
#6710=ADVANCED_FACE('',(#831),#666,.T.);
#6711=ADVANCED_FACE('',(#832),#667,.T.);
#6712=ADVANCED_FACE('',(#833),#668,.T.);
#6713=ADVANCED_FACE('',(#834),#669,.T.);
#6714=ADVANCED_FACE('',(#835),#670,.T.);
#6715=ADVANCED_FACE('',(#836),#6563,.T.);
#6716=ADVANCED_FACE('',(#837),#6564,.T.);
#6717=ADVANCED_FACE('',(#838,#589,#590,#591,#592),#671,.T.);
#6718=ADVANCED_FACE('',(#839),#585,.T.);
#6719=ADVANCED_FACE('',(#840),#6565,.F.);
#6720=ADVANCED_FACE('',(#841,#593,#594,#595,#596),#672,.F.);
#6721=ADVANCED_FACE('',(#842),#586,.T.);
#6722=ADVANCED_FACE('',(#843),#6566,.T.);
#6723=ADVANCED_FACE('',(#844),#6567,.T.);
#6724=ADVANCED_FACE('',(#845),#673,.T.);
#6725=ADVANCED_FACE('',(#846),#674,.T.);
#6726=ADVANCED_FACE('',(#847),#675,.T.);
#6727=ADVANCED_FACE('',(#848),#676,.T.);
#6728=ADVANCED_FACE('',(#849),#677,.T.);
#6729=ADVANCED_FACE('',(#850),#678,.T.);
#6730=ADVANCED_FACE('',(#851),#679,.T.);
#6731=ADVANCED_FACE('',(#852),#680,.T.);
#6732=ADVANCED_FACE('',(#853),#6568,.F.);
#6733=ADVANCED_FACE('',(#854),#6569,.F.);
#6734=ADVANCED_FACE('',(#855),#6570,.F.);
#6735=ADVANCED_FACE('',(#856),#681,.T.);
#6736=ADVANCED_FACE('',(#857),#682,.T.);
#6737=ADVANCED_FACE('',(#858),#6571,.T.);
#6738=ADVANCED_FACE('',(#859),#6572,.T.);
#6739=ADVANCED_FACE('',(#860),#6573,.T.);
#6740=ADVANCED_FACE('',(#861),#683,.T.);
#6741=ADVANCED_FACE('',(#862),#684,.T.);
#6742=ADVANCED_FACE('',(#863),#685,.T.);
#6743=ADVANCED_FACE('',(#864),#686,.T.);
#6744=ADVANCED_FACE('',(#865),#687,.T.);
#6745=ADVANCED_FACE('',(#866),#6574,.T.);
#6746=ADVANCED_FACE('',(#867),#6575,.T.);
#6747=ADVANCED_FACE('',(#868,#597,#598,#599,#600),#688,.T.);
#6748=ADVANCED_FACE('',(#869),#587,.T.);
#6749=ADVANCED_FACE('',(#870),#6576,.F.);
#6750=ADVANCED_FACE('',(#871,#601,#602,#603,#604),#689,.F.);
#6751=ADVANCED_FACE('',(#872),#588,.T.);
#6752=ADVANCED_FACE('',(#873),#6577,.T.);
#6753=ADVANCED_FACE('',(#874),#6578,.T.);
#6754=ADVANCED_FACE('',(#875),#690,.T.);
#6755=ADVANCED_FACE('',(#876),#691,.T.);
#6756=ADVANCED_FACE('',(#877),#692,.T.);
#6757=ADVANCED_FACE('',(#878),#693,.T.);
#6758=ADVANCED_FACE('',(#879),#694,.T.);
#6759=ADVANCED_FACE('',(#880),#695,.T.);
#6760=ADVANCED_FACE('',(#881),#696,.T.);
#6761=ADVANCED_FACE('',(#882),#697,.T.);
#6762=ADVANCED_FACE('',(#883),#6579,.T.);
#6763=ADVANCED_FACE('',(#884,#605),#698,.F.);
#6764=ADVANCED_FACE('',(#885,#606),#699,.F.);
#6765=ADVANCED_FACE('',(#886),#6580,.T.);
#6766=ADVANCED_FACE('',(#887,#607),#700,.T.);
#6767=ADVANCED_FACE('',(#888),#6581,.T.);
#6768=ADVANCED_FACE('',(#889),#701,.F.);
#6769=ADVANCED_FACE('',(#890),#6582,.T.);
#6770=ADVANCED_FACE('',(#891),#702,.T.);
#6771=ADVANCED_FACE('',(#892),#703,.F.);
#6772=ADVANCED_FACE('',(#893),#704,.F.);
#6773=ADVANCED_FACE('',(#894),#705,.F.);
#6774=ADVANCED_FACE('',(#895),#6583,.F.);
#6775=ADVANCED_FACE('',(#896),#6584,.T.);
#6776=ADVANCED_FACE('',(#897),#706,.T.);
#6777=ADVANCED_FACE('',(#898,#608,#609,#610),#707,.F.);
#6778=ADVANCED_FACE('',(#899),#6585,.F.);
#6779=ADVANCED_FACE('',(#900),#6586,.F.);
#6780=ADVANCED_FACE('',(#901),#6587,.F.);
#6781=ADVANCED_FACE('',(#902),#6588,.F.);
#6782=ADVANCED_FACE('',(#903),#6589,.F.);
#6783=ADVANCED_FACE('',(#904,#611),#708,.F.);
#6784=ADVANCED_FACE('',(#905),#6590,.F.);
#6785=ADVANCED_FACE('',(#906,#612),#709,.F.);
#6786=ADVANCED_FACE('',(#907),#6591,.F.);
#6787=ADVANCED_FACE('',(#908),#6592,.F.);
#6788=ADVANCED_FACE('',(#909),#710,.F.);
#6789=ADVANCED_FACE('',(#910),#711,.F.);
#6790=ADVANCED_FACE('',(#911),#712,.F.);
#6791=ADVANCED_FACE('',(#912),#713,.F.);
#6792=ADVANCED_FACE('',(#913),#714,.F.);
#6793=ADVANCED_FACE('',(#914),#715,.F.);
#6794=ADVANCED_FACE('',(#915),#716,.F.);
#6795=ADVANCED_FACE('',(#916,#613),#717,.F.);
#6796=ADVANCED_FACE('',(#917,#614),#718,.F.);
#6797=ADVANCED_FACE('',(#918),#719,.F.);
#6798=ADVANCED_FACE('',(#919),#720,.F.);
#6799=ADVANCED_FACE('',(#920),#721,.F.);
#6800=ADVANCED_FACE('',(#921),#722,.F.);
#6801=ADVANCED_FACE('',(#922),#723,.F.);
#6802=ADVANCED_FACE('',(#923),#724,.T.);
#6803=ADVANCED_FACE('',(#924),#725,.T.);
#6804=ADVANCED_FACE('',(#925),#726,.T.);
#6805=ADVANCED_FACE('',(#926),#727,.T.);
#6806=ADVANCED_FACE('',(#927),#728,.T.);
#6807=ADVANCED_FACE('',(#928,#615),#729,.F.);
#6808=ADVANCED_FACE('',(#929),#6593,.T.);
#6809=ADVANCED_FACE('',(#930),#6594,.T.);
#6810=ADVANCED_FACE('',(#931),#730,.T.);
#6811=ADVANCED_FACE('',(#932),#91,.T.);
#6812=ADVANCED_FACE('',(#933),#92,.T.);
#6813=ADVANCED_FACE('',(#934),#93,.T.);
#6814=ADVANCED_FACE('',(#935),#94,.T.);
#6815=ADVANCED_FACE('',(#936,#616,#617,#618),#731,.F.);
#6816=ADVANCED_FACE('',(#937),#732,.F.);
#6817=ADVANCED_FACE('',(#938),#95,.T.);
#6818=ADVANCED_FACE('',(#939),#96,.T.);
#6819=ADVANCED_FACE('',(#940),#97,.T.);
#6820=ADVANCED_FACE('',(#941),#733,.T.);
#6821=ADVANCED_FACE('',(#942),#98,.T.);
#6822=ADVANCED_FACE('',(#943),#99,.T.);
#6823=ADVANCED_FACE('',(#944),#734,.F.);
#6824=ADVANCED_FACE('',(#945),#100,.T.);
#6825=ADVANCED_FACE('',(#946),#101,.T.);
#6826=ADVANCED_FACE('',(#947),#735,.T.);
#6827=ADVANCED_FACE('',(#948),#102,.T.);
#6828=ADVANCED_FACE('',(#949),#103,.T.);
#6829=ADVANCED_FACE('',(#950),#104,.T.);
#6830=ADVANCED_FACE('',(#951),#105,.T.);
#6831=ADVANCED_FACE('',(#952),#736,.T.);
#6832=ADVANCED_FACE('',(#953),#106,.T.);
#6833=ADVANCED_FACE('',(#954),#107,.T.);
#6834=ADVANCED_FACE('',(#955),#737,.F.);
#6835=ADVANCED_FACE('',(#956),#108,.T.);
#6836=ADVANCED_FACE('',(#957),#109,.T.);
#6837=ADVANCED_FACE('',(#958),#75,.F.);
#6838=ADVANCED_FACE('',(#959),#76,.F.);
#6839=ADVANCED_FACE('',(#960),#77,.F.);
#6840=ADVANCED_FACE('',(#961),#6595,.F.);
#6841=ADVANCED_FACE('',(#962),#110,.T.);
#6842=ADVANCED_FACE('',(#963),#78,.F.);
#6843=ADVANCED_FACE('',(#964),#6596,.F.);
#6844=ADVANCED_FACE('',(#965),#111,.T.);
#6845=ADVANCED_FACE('',(#966),#112,.T.);
#6846=ADVANCED_FACE('',(#967),#113,.T.);
#6847=ADVANCED_FACE('',(#968),#114,.T.);
#6848=ADVANCED_FACE('',(#969),#738,.T.);
#6849=ADVANCED_FACE('',(#970),#79,.T.);
#6850=ADVANCED_FACE('',(#971),#80,.T.);
#6851=ADVANCED_FACE('',(#972),#81,.T.);
#6852=ADVANCED_FACE('',(#973),#6597,.T.);
#6853=ADVANCED_FACE('',(#974),#115,.F.);
#6854=ADVANCED_FACE('',(#975),#82,.T.);
#6855=ADVANCED_FACE('',(#976),#6598,.T.);
#6856=ADVANCED_FACE('',(#977),#116,.F.);
#6857=ADVANCED_FACE('',(#978),#117,.F.);
#6858=ADVANCED_FACE('',(#979),#118,.F.);
#6859=ADVANCED_FACE('',(#980),#119,.F.);
#6860=ADVANCED_FACE('',(#981),#120,.F.);
#6861=ADVANCED_FACE('',(#982),#121,.F.);
#6862=ADVANCED_FACE('',(#983),#739,.F.);
#6863=ADVANCED_FACE('',(#984,#619,#620,#621,#622,#623,#624),#740,.T.);
#6864=ADVANCED_FACE('',(#985),#122,.F.);
#6865=ADVANCED_FACE('',(#986),#741,.F.);
#6866=ADVANCED_FACE('',(#987,#625,#626,#627),#742,.F.);
#6867=ADVANCED_FACE('',(#988),#6599,.F.);
#6868=ADVANCED_FACE('',(#989),#6600,.F.);
#6869=ADVANCED_FACE('',(#990),#6601,.F.);
#6870=ADVANCED_FACE('',(#991),#6602,.F.);
#6871=ADVANCED_FACE('',(#992),#743,.F.);
#6872=ADVANCED_FACE('',(#993),#744,.F.);
#6873=ADVANCED_FACE('',(#994),#745,.F.);
#6874=ADVANCED_FACE('',(#995),#746,.F.);
#6875=ADVANCED_FACE('',(#996),#747,.F.);
#6876=ADVANCED_FACE('',(#997),#748,.F.);
#6877=ADVANCED_FACE('',(#998,#628),#749,.F.);
#6878=ADVANCED_FACE('',(#999),#750,.F.);
#6879=ADVANCED_FACE('',(#1000),#751,.F.);
#6880=ADVANCED_FACE('',(#1001),#752,.F.);
#6881=ADVANCED_FACE('',(#1002),#753,.F.);
#6882=ADVANCED_FACE('',(#1003),#754,.F.);
#6883=ADVANCED_FACE('',(#1004),#755,.F.);
#6884=ADVANCED_FACE('',(#1005,#629),#756,.F.);
#6885=ADVANCED_FACE('',(#1006),#6603,.F.);
#6886=ADVANCED_FACE('',(#1007),#6604,.F.);
#6887=ADVANCED_FACE('',(#1008),#757,.F.);
#6888=ADVANCED_FACE('',(#1009),#758,.F.);
#6889=ADVANCED_FACE('',(#1010),#759,.F.);
#6890=ADVANCED_FACE('',(#1011),#760,.F.);
#6891=ADVANCED_FACE('',(#1012),#761,.F.);
#6892=ADVANCED_FACE('',(#1013),#762,.F.);
#6893=ADVANCED_FACE('',(#1014),#763,.F.);
#6894=ADVANCED_FACE('',(#1015,#630),#764,.F.);
#6895=ADVANCED_FACE('',(#1016,#631),#765,.F.);
#6896=ADVANCED_FACE('',(#1017),#766,.F.);
#6897=ADVANCED_FACE('',(#1018),#767,.F.);
#6898=ADVANCED_FACE('',(#1019),#768,.F.);
#6899=ADVANCED_FACE('',(#1020),#769,.F.);
#6900=ADVANCED_FACE('',(#1021),#770,.F.);
#6901=ADVANCED_FACE('',(#1022),#771,.T.);
#6902=ADVANCED_FACE('',(#1023),#772,.T.);
#6903=ADVANCED_FACE('',(#1024),#773,.T.);
#6904=ADVANCED_FACE('',(#1025),#774,.T.);
#6905=ADVANCED_FACE('',(#1026),#775,.T.);
#6906=ADVANCED_FACE('',(#1027,#632),#776,.F.);
#6907=ADVANCED_FACE('',(#1028),#6605,.T.);
#6908=ADVANCED_FACE('',(#1029),#6606,.T.);
#6909=ADVANCED_FACE('',(#1030),#777,.T.);
#6910=ADVANCED_FACE('',(#1031),#123,.T.);
#6911=ADVANCED_FACE('',(#1032),#124,.T.);
#6912=ADVANCED_FACE('',(#1033),#125,.T.);
#6913=ADVANCED_FACE('',(#1034),#126,.T.);
#6914=ADVANCED_FACE('',(#1035,#633,#634,#635),#778,.F.);
#6915=ADVANCED_FACE('',(#1036),#779,.F.);
#6916=ADVANCED_FACE('',(#1037),#127,.T.);
#6917=ADVANCED_FACE('',(#1038),#128,.T.);
#6918=ADVANCED_FACE('',(#1039),#129,.T.);
#6919=ADVANCED_FACE('',(#1040),#780,.T.);
#6920=ADVANCED_FACE('',(#1041),#130,.T.);
#6921=ADVANCED_FACE('',(#1042),#131,.T.);
#6922=ADVANCED_FACE('',(#1043),#781,.F.);
#6923=ADVANCED_FACE('',(#1044),#132,.T.);
#6924=ADVANCED_FACE('',(#1045),#133,.T.);
#6925=ADVANCED_FACE('',(#1046),#782,.T.);
#6926=ADVANCED_FACE('',(#1047),#134,.T.);
#6927=ADVANCED_FACE('',(#1048),#135,.T.);
#6928=ADVANCED_FACE('',(#1049),#136,.T.);
#6929=ADVANCED_FACE('',(#1050),#137,.T.);
#6930=ADVANCED_FACE('',(#1051),#783,.T.);
#6931=ADVANCED_FACE('',(#1052),#138,.T.);
#6932=ADVANCED_FACE('',(#1053),#139,.T.);
#6933=ADVANCED_FACE('',(#1054),#784,.F.);
#6934=ADVANCED_FACE('',(#1055),#140,.T.);
#6935=ADVANCED_FACE('',(#1056),#141,.T.);
#6936=ADVANCED_FACE('',(#1057),#83,.F.);
#6937=ADVANCED_FACE('',(#1058),#84,.F.);
#6938=ADVANCED_FACE('',(#1059),#85,.F.);
#6939=ADVANCED_FACE('',(#1060),#6607,.F.);
#6940=ADVANCED_FACE('',(#1061),#142,.T.);
#6941=ADVANCED_FACE('',(#1062),#86,.F.);
#6942=ADVANCED_FACE('',(#1063),#6608,.F.);
#6943=ADVANCED_FACE('',(#1064),#143,.T.);
#6944=ADVANCED_FACE('',(#1065),#144,.T.);
#6945=ADVANCED_FACE('',(#1066),#145,.T.);
#6946=ADVANCED_FACE('',(#1067),#146,.T.);
#6947=ADVANCED_FACE('',(#1068),#785,.T.);
#6948=ADVANCED_FACE('',(#1069),#87,.T.);
#6949=ADVANCED_FACE('',(#1070),#88,.T.);
#6950=ADVANCED_FACE('',(#1071),#89,.T.);
#6951=ADVANCED_FACE('',(#1072),#6609,.T.);
#6952=ADVANCED_FACE('',(#1073),#147,.F.);
#6953=ADVANCED_FACE('',(#1074),#90,.T.);
#6954=ADVANCED_FACE('',(#1075),#6610,.T.);
#6955=ADVANCED_FACE('',(#1076),#148,.F.);
#6956=ADVANCED_FACE('',(#1077),#149,.F.);
#6957=ADVANCED_FACE('',(#1078),#150,.F.);
#6958=ADVANCED_FACE('',(#1079),#151,.F.);
#6959=ADVANCED_FACE('',(#1080),#152,.F.);
#6960=ADVANCED_FACE('',(#1081),#153,.F.);
#6961=ADVANCED_FACE('',(#1082),#786,.F.);
#6962=ADVANCED_FACE('',(#1083,#636,#637,#638,#639,#640,#641),#787,.T.);
#6963=ADVANCED_FACE('',(#1084),#154,.F.);
#6964=ADVANCED_FACE('',(#1085),#788,.F.);
#6965=ADVANCED_FACE('',(#1086),#6611,.F.);
#6966=ADVANCED_FACE('',(#1087),#6612,.F.);
#6967=ADVANCED_FACE('',(#1088,#642),#789,.T.);
#6968=ADVANCED_FACE('',(#1089),#6613,.T.);
#6969=ADVANCED_FACE('',(#1090),#790,.F.);
#6970=ADVANCED_FACE('',(#1091,#643),#791,.T.);
#6971=ADVANCED_FACE('',(#1092),#6614,.T.);
#6972=ADVANCED_FACE('',(#1093),#792,.F.);
#6973=ADVANCED_FACE('',(#1094,#644),#793,.T.);
#6974=ADVANCED_FACE('',(#1095),#6615,.T.);
#6975=ADVANCED_FACE('',(#1096),#794,.F.);
#6976=ADVANCED_FACE('',(#1097,#645),#795,.T.);
#6977=ADVANCED_FACE('',(#1098),#6616,.T.);
#6978=ADVANCED_FACE('',(#1099),#796,.F.);
#6979=ADVANCED_FACE('',(#1100),#6617,.T.);
#6980=ADVANCED_FACE('',(#1101),#6618,.T.);
#6981=ADVANCED_FACE('',(#1102),#6619,.T.);
#6982=ADVANCED_FACE('',(#1103),#6620,.T.);
#6983=ADVANCED_FACE('',(#1104),#155,.F.);
#6984=ADVANCED_FACE('',(#1105),#6621,.T.);
#6985=ADVANCED_FACE('',(#1106),#156,.F.);
#6986=ADVANCED_FACE('',(#1107),#157,.F.);
#6987=ADVANCED_FACE('',(#1108),#158,.F.);
#6988=ADVANCED_FACE('',(#1109),#6622,.T.);
#6989=ADVANCED_FACE('',(#1110),#159,.F.);
#6990=ADVANCED_FACE('',(#1111),#160,.F.);
#6991=ADVANCED_FACE('',(#1112),#797,.F.);
#6992=ADVANCED_FACE('',(#1113),#161,.F.);
#6993=ADVANCED_FACE('',(#1114),#162,.F.);
#6994=ADVANCED_FACE('',(#1115),#163,.F.);
#6995=ADVANCED_FACE('',(#1116,#646,#647),#798,.T.);
#6996=ADVANCED_FACE('',(#1117),#799,.F.);
#6997=ADVANCED_FACE('',(#1118),#164,.F.);
#6998=ADVANCED_FACE('',(#1119),#165,.F.);
#6999=ADVANCED_FACE('',(#1120,#648,#649,#650,#651,#652,#653),#800,.F.);
#7000=ADVANCED_FACE('',(#1121),#166,.F.);
#7001=ADVANCED_FACE('',(#1122),#6623,.T.);
#7002=ADVANCED_FACE('',(#1123),#6624,.T.);
#7003=ADVANCED_FACE('',(#1124),#6625,.T.);
#7004=ADVANCED_FACE('',(#1125),#6626,.T.);
#7005=ADVANCED_FACE('',(#1126),#6627,.T.);
#7006=ADVANCED_FACE('',(#1127),#6628,.T.);
#7007=ADVANCED_FACE('',(#1128),#6629,.T.);
#7008=ADVANCED_FACE('',(#1129),#6630,.T.);
#7009=ADVANCED_FACE('',(#1130),#6631,.T.);
#7010=ADVANCED_FACE('',(#1131),#6632,.T.);
#7011=ADVANCED_FACE('',(#1132),#6633,.T.);
#7012=ADVANCED_FACE('',(#1133),#6634,.T.);
#7013=ADVANCED_FACE('',(#1134),#6635,.T.);
#7014=ADVANCED_FACE('',(#1135),#6636,.T.);
#7015=ADVANCED_FACE('',(#1136),#6637,.T.);
#7016=ADVANCED_FACE('',(#1137),#6638,.T.);
#7017=ADVANCED_FACE('',(#1138),#6639,.T.);
#7018=ADVANCED_FACE('',(#1139),#6640,.T.);
#7019=ADVANCED_FACE('',(#1140),#6641,.T.);
#7020=ADVANCED_FACE('',(#1141),#6642,.T.);
#7021=ADVANCED_FACE('',(#1142),#6643,.T.);
#7022=ADVANCED_FACE('',(#1143),#6644,.T.);
#7023=ADVANCED_FACE('',(#1144),#6645,.T.);
#7024=ADVANCED_FACE('',(#1145),#6646,.T.);
#7025=ADVANCED_FACE('',(#1146),#6647,.T.);
#7026=ADVANCED_FACE('',(#1147),#6648,.T.);
#7027=ADVANCED_FACE('',(#1148),#6649,.T.);
#7028=ADVANCED_FACE('',(#1149),#6650,.T.);
#7029=ADVANCED_FACE('',(#1150),#6651,.T.);
#7030=ADVANCED_FACE('',(#1151),#6652,.T.);
#7031=ADVANCED_FACE('',(#1152),#6653,.T.);
#7032=ADVANCED_FACE('',(#1153),#6654,.T.);
#7033=ADVANCED_FACE('',(#1154),#6655,.T.);
#7034=ADVANCED_FACE('',(#1155),#6656,.T.);
#7035=ADVANCED_FACE('',(#1156),#6657,.T.);
#7036=ADVANCED_FACE('',(#1157),#6658,.T.);
#7037=ADVANCED_FACE('',(#1158),#6659,.T.);
#7038=ADVANCED_FACE('',(#1159),#6660,.T.);
#7039=ADVANCED_FACE('',(#1160),#6661,.T.);
#7040=ADVANCED_FACE('',(#1161),#6662,.T.);
#7041=ADVANCED_FACE('',(#1162),#6663,.T.);
#7042=ADVANCED_FACE('',(#1163),#6664,.T.);
#7043=ADVANCED_FACE('',(#1164),#6665,.T.);
#7044=ADVANCED_FACE('',(#1165),#6666,.T.);
#7045=ADVANCED_FACE('',(#1166),#6667,.T.);
#7046=ADVANCED_FACE('',(#1167),#6668,.T.);
#7047=ADVANCED_FACE('',(#1168),#6669,.T.);
#7048=ADVANCED_FACE('',(#1169),#6670,.T.);
#7049=ADVANCED_FACE('',(#1170),#6671,.T.);
#7050=ADVANCED_FACE('',(#1171),#6672,.T.);
#7051=ADVANCED_FACE('',(#1172),#6673,.T.);
#7052=ADVANCED_FACE('',(#1173),#6674,.T.);
#7053=ADVANCED_FACE('',(#1174),#6675,.T.);
#7054=ADVANCED_FACE('',(#1175),#6676,.T.);
#7055=ADVANCED_FACE('',(#1176),#6677,.T.);
#7056=ADVANCED_FACE('',(#1177),#6678,.T.);
#7057=ADVANCED_FACE('',(#1178),#6679,.T.);
#7058=ADVANCED_FACE('',(#1179),#6680,.T.);
#7059=ADVANCED_FACE('',(#1180),#6681,.T.);
#7060=ADVANCED_FACE('',(#1181),#6682,.T.);
#7061=ADVANCED_FACE('',(#1182),#661,.T.);
#7062=ADVANCED_FACE('',(#1183),#167,.F.);
#7063=ADVANCED_FACE('',(#1184),#6683,.T.);
#7064=ADVANCED_FACE('',(#1185),#168,.F.);
#7065=ADVANCED_FACE('',(#1186),#6684,.T.);
#7066=ADVANCED_FACE('',(#1187),#801,.F.);
#7067=ADVANCED_FACE('',(#1188),#802,.F.);
#7068=ADVANCED_FACE('',(#1189),#803,.F.);
#7069=ADVANCED_FACE('',(#1190),#804,.F.);
#7070=ADVANCED_FACE('',(#1191),#805,.F.);
#7071=ADVANCED_FACE('',(#1192),#806,.F.);
#7072=ADVANCED_FACE('',(#1193),#807,.F.);
#7073=ADVANCED_FACE('',(#1194,#654),#808,.T.);
#7074=ADVANCED_FACE('',(#1195),#6685,.T.);
#7075=ADVANCED_FACE('',(#1196,#655),#809,.F.);
#7076=ADVANCED_FACE('',(#1197),#810,.T.);
#7077=ADVANCED_FACE('',(#1198),#6686,.F.);
#7078=ADVANCED_FACE('',(#1199),#6687,.F.);
#7079=ADVANCED_FACE('',(#1200),#6688,.F.);
#7080=ADVANCED_FACE('',(#1201),#6689,.F.);
#7081=ADVANCED_FACE('',(#1202),#6690,.F.);
#7082=ADVANCED_FACE('',(#1203),#6691,.F.);
#7083=ADVANCED_FACE('',(#1204),#6692,.F.);
#7084=ADVANCED_FACE('',(#1205),#6693,.F.);
#7085=ADVANCED_FACE('',(#1206),#6694,.F.);
#7086=ADVANCED_FACE('',(#1207),#6695,.F.);
#7087=ADVANCED_FACE('',(#1208),#6696,.F.);
#7088=ADVANCED_FACE('',(#1209),#169,.F.);
#7089=ADVANCED_FACE('',(#1210),#170,.F.);
#7090=ADVANCED_FACE('',(#1211,#656),#811,.T.);
#7091=ADVANCED_FACE('',(#1212),#6697,.F.);
#7092=ADVANCED_FACE('',(#1213),#812,.T.);
#7093=ADVANCED_FACE('',(#1214),#813,.T.);
#7094=ADVANCED_FACE('',(#1215),#814,.T.);
#7095=ADVANCED_FACE('',(#1216),#815,.T.);
#7096=ADVANCED_FACE('',(#1217),#816,.T.);
#7097=ADVANCED_FACE('',(#1218),#817,.T.);
#7098=ADVANCED_FACE('',(#1219,#657),#818,.F.);
#7099=ADVANCED_FACE('',(#1220),#6698,.F.);
#7100=ADVANCED_FACE('',(#1221),#6699,.T.);
#7101=ADVANCED_FACE('',(#1222,#658),#819,.T.);
#7102=ADVANCED_FACE('',(#1223,#659),#820,.F.);
#7103=CLOSED_SHELL('',(#6700,#6701,#6702,#6703,#6704,#6705,#6706,#6707,
#6708,#6709,#6710,#6711,#6712,#6713,#6714,#6715,#6716,#6717,#6718,#6719,
#6720,#6721,#6722,#6723,#6724,#6725,#6726,#6727,#6728,#6729,#6730,#6731));
#7104=CLOSED_SHELL('',(#6732,#6733,#6734,#6735,#6736,#6737,#6738,#6739,
#6740,#6741,#6742,#6743,#6744,#6745,#6746,#6747,#6748,#6749,#6750,#6751,
#6752,#6753,#6754,#6755,#6756,#6757,#6758,#6759,#6760,#6761));
#7105=CLOSED_SHELL('',(#6762,#6763,#6764,#6765,#6766,#6767,#6768,#6769,
#6770));
#7106=CLOSED_SHELL('',(#6771,#6772,#6773,#6774,#6775,#6776));
#7107=CLOSED_SHELL('',(#6777,#6778,#6779,#6780,#6781,#6782,#6783,#6784,
#6785,#6786,#6787,#6788,#6789,#6790,#6791,#6792,#6793,#6794,#6795,#6796,
#6797,#6798,#6799,#6800,#6801,#6802,#6803,#6804,#6805,#6806,#6807,#6808,
#6809,#6810,#6811,#6812,#6813,#6814,#6815,#6816,#6817,#6818,#6819,#6820,
#6821,#6822,#6823,#6824,#6825,#6826,#6827,#6828,#6829,#6830,#6831,#6832,
#6833,#6834,#6835,#6836,#6837,#6838,#6839,#6840,#6841,#6842,#6843,#6844,
#6845,#6846,#6847,#6848,#6849,#6850,#6851,#6852,#6853,#6854,#6855,#6856,
#6857,#6858,#6859,#6860,#6861,#6862,#6863,#6864,#6865));
#7108=CLOSED_SHELL('',(#6866,#6867,#6868,#6869,#6870,#6871,#6872,#6873,
#6874,#6875,#6876,#6877,#6878,#6879,#6880,#6881,#6882,#6883,#6884,#6885,
#6886,#6887,#6888,#6889,#6890,#6891,#6892,#6893,#6894,#6895,#6896,#6897,
#6898,#6899,#6900,#6901,#6902,#6903,#6904,#6905,#6906,#6907,#6908,#6909,
#6910,#6911,#6912,#6913,#6914,#6915,#6916,#6917,#6918,#6919,#6920,#6921,
#6922,#6923,#6924,#6925,#6926,#6927,#6928,#6929,#6930,#6931,#6932,#6933,
#6934,#6935,#6936,#6937,#6938,#6939,#6940,#6941,#6942,#6943,#6944,#6945,
#6946,#6947,#6948,#6949,#6950,#6951,#6952,#6953,#6954,#6955,#6956,#6957,
#6958,#6959,#6960,#6961,#6962,#6963,#6964));
#7109=CLOSED_SHELL('',(#6965,#6966,#6967,#6968,#6969,#6970,#6971,#6972,
#6973,#6974,#6975,#6976,#6977,#6978,#6979,#6980,#6981,#6982,#6983,#6984,
#6985,#6986,#6987,#6988,#6989,#6990,#6991,#6992,#6993,#6994,#6995,#6996,
#6997,#6998,#6999,#7000));
#7110=CLOSED_SHELL('',(#7001,#7002,#7003,#7004,#7005,#7006,#7007,#7008,
#7009,#7010,#7011,#7012,#7013,#7014,#7015,#7016,#7017,#7018,#7019,#7020,
#7021,#7022,#7023,#7024,#7025,#7026,#7027,#7028,#7029,#7030,#7031,#7032,
#7033,#7034,#7035,#7036,#7037,#7038,#7039,#7040,#7041,#7042,#7043,#7044,
#7045,#7046,#7047,#7048,#7049,#7050,#7051,#7052,#7053,#7054,#7055,#7056,
#7057,#7058,#7059,#7060,#7061,#7062,#7063,#7064,#7065,#7066,#7067,#7068,
#7069,#7070,#7071,#7072,#7073,#7074,#7075,#7076));
#7111=CLOSED_SHELL('',(#7077,#7078,#7079,#7080,#7081,#7082,#7083,#7084,
#7085,#7086,#7087,#7088,#7089,#7090,#7091,#7092,#7093,#7094,#7095,#7096,
#7097,#7098));
#7112=CLOSED_SHELL('',(#7099,#7100,#7101,#7102));
#7113=DERIVED_UNIT_ELEMENT(#7133,1.);
#7114=DERIVED_UNIT_ELEMENT(#19620,-3.);
#7115=DERIVED_UNIT_ELEMENT(#7133,1.);
#7116=DERIVED_UNIT_ELEMENT(#19620,-3.);
#7117=DERIVED_UNIT_ELEMENT(#7133,1.);
#7118=DERIVED_UNIT_ELEMENT(#19620,-3.);
#7119=DERIVED_UNIT_ELEMENT(#7133,1.);
#7120=DERIVED_UNIT_ELEMENT(#19620,-3.);
#7121=DERIVED_UNIT_ELEMENT(#7133,1.);
#7122=DERIVED_UNIT_ELEMENT(#19620,-3.);
#7123=DERIVED_UNIT_ELEMENT(#7133,1.);
#7124=DERIVED_UNIT_ELEMENT(#19620,-3.);
#7125=DERIVED_UNIT_ELEMENT(#7133,1.);
#7126=DERIVED_UNIT_ELEMENT(#19620,-3.);
#7127=DERIVED_UNIT_ELEMENT(#7133,1.);
#7128=DERIVED_UNIT_ELEMENT(#19620,-3.);
#7129=DERIVED_UNIT_ELEMENT(#7133,1.);
#7130=DERIVED_UNIT_ELEMENT(#19620,-3.);
#7131=DERIVED_UNIT_ELEMENT(#7133,1.);
#7132=DERIVED_UNIT_ELEMENT(#19620,-3.);
#7133=(
MASS_UNIT()
NAMED_UNIT(*)
SI_UNIT(.KILO.,.GRAM.)
);
#7134=DERIVED_UNIT((#7113,#7114));
#7135=DERIVED_UNIT((#7115,#7116));
#7136=DERIVED_UNIT((#7117,#7118));
#7137=DERIVED_UNIT((#7119,#7120));
#7138=DERIVED_UNIT((#7121,#7122));
#7139=DERIVED_UNIT((#7123,#7124));
#7140=DERIVED_UNIT((#7125,#7126));
#7141=DERIVED_UNIT((#7127,#7128));
#7142=DERIVED_UNIT((#7129,#7130));
#7143=DERIVED_UNIT((#7131,#7132));
#7144=MEASURE_REPRESENTATION_ITEM('density measure',
POSITIVE_RATIO_MEASURE(7850.),#7134);
#7145=MEASURE_REPRESENTATION_ITEM('density measure',
POSITIVE_RATIO_MEASURE(7850.),#7135);
#7146=MEASURE_REPRESENTATION_ITEM('density measure',
POSITIVE_RATIO_MEASURE(7850.),#7136);
#7147=MEASURE_REPRESENTATION_ITEM('density measure',
POSITIVE_RATIO_MEASURE(7850.),#7137);
#7148=MEASURE_REPRESENTATION_ITEM('density measure',
POSITIVE_RATIO_MEASURE(7850.),#7138);
#7149=MEASURE_REPRESENTATION_ITEM('density measure',
POSITIVE_RATIO_MEASURE(7850.),#7139);
#7150=MEASURE_REPRESENTATION_ITEM('density measure',
POSITIVE_RATIO_MEASURE(7850.),#7140);
#7151=MEASURE_REPRESENTATION_ITEM('density measure',
POSITIVE_RATIO_MEASURE(7850.),#7141);
#7152=MEASURE_REPRESENTATION_ITEM('density measure',
POSITIVE_RATIO_MEASURE(7850.),#7142);
#7153=MEASURE_REPRESENTATION_ITEM('density measure',
POSITIVE_RATIO_MEASURE(7850.),#7143);
#7154=PROPERTY_DEFINITION_REPRESENTATION(#7204,#7174);
#7155=PROPERTY_DEFINITION_REPRESENTATION(#7205,#7175);
#7156=PROPERTY_DEFINITION_REPRESENTATION(#7206,#7176);
#7157=PROPERTY_DEFINITION_REPRESENTATION(#7207,#7177);
#7158=PROPERTY_DEFINITION_REPRESENTATION(#7208,#7178);
#7159=PROPERTY_DEFINITION_REPRESENTATION(#7209,#7179);
#7160=PROPERTY_DEFINITION_REPRESENTATION(#7210,#7180);
#7161=PROPERTY_DEFINITION_REPRESENTATION(#7211,#7181);
#7162=PROPERTY_DEFINITION_REPRESENTATION(#7212,#7182);
#7163=PROPERTY_DEFINITION_REPRESENTATION(#7213,#7183);
#7164=PROPERTY_DEFINITION_REPRESENTATION(#7214,#7184);
#7165=PROPERTY_DEFINITION_REPRESENTATION(#7215,#7185);
#7166=PROPERTY_DEFINITION_REPRESENTATION(#7216,#7186);
#7167=PROPERTY_DEFINITION_REPRESENTATION(#7217,#7187);
#7168=PROPERTY_DEFINITION_REPRESENTATION(#7218,#7188);
#7169=PROPERTY_DEFINITION_REPRESENTATION(#7219,#7189);
#7170=PROPERTY_DEFINITION_REPRESENTATION(#7220,#7190);
#7171=PROPERTY_DEFINITION_REPRESENTATION(#7221,#7191);
#7172=PROPERTY_DEFINITION_REPRESENTATION(#7222,#7192);
#7173=PROPERTY_DEFINITION_REPRESENTATION(#7223,#7193);
#7174=REPRESENTATION('material name',(#7194),#19607);
#7175=REPRESENTATION('density',(#7144),#19607);
#7176=REPRESENTATION('material name',(#7195),#19608);
#7177=REPRESENTATION('density',(#7145),#19608);
#7178=REPRESENTATION('material name',(#7196),#19609);
#7179=REPRESENTATION('density',(#7146),#19609);
#7180=REPRESENTATION('material name',(#7197),#19610);
#7181=REPRESENTATION('density',(#7147),#19610);
#7182=REPRESENTATION('material name',(#7198),#19612);
#7183=REPRESENTATION('density',(#7148),#19612);
#7184=REPRESENTATION('material name',(#7199),#19613);
#7185=REPRESENTATION('density',(#7149),#19613);
#7186=REPRESENTATION('material name',(#7200),#19614);
#7187=REPRESENTATION('density',(#7150),#19614);
#7188=REPRESENTATION('material name',(#7201),#19615);
#7189=REPRESENTATION('density',(#7151),#19615);
#7190=REPRESENTATION('material name',(#7202),#19616);
#7191=REPRESENTATION('density',(#7152),#19616);
#7192=REPRESENTATION('material name',(#7203),#19617);
#7193=REPRESENTATION('density',(#7153),#19617);
#7194=DESCRIPTIVE_REPRESENTATION_ITEM('Steel','Steel');
#7195=DESCRIPTIVE_REPRESENTATION_ITEM('Steel','Steel');
#7196=DESCRIPTIVE_REPRESENTATION_ITEM('Steel','Steel');
#7197=DESCRIPTIVE_REPRESENTATION_ITEM('Steel','Steel');
#7198=DESCRIPTIVE_REPRESENTATION_ITEM('Steel','Steel');
#7199=DESCRIPTIVE_REPRESENTATION_ITEM('Steel','Steel');
#7200=DESCRIPTIVE_REPRESENTATION_ITEM('Steel','Steel');
#7201=DESCRIPTIVE_REPRESENTATION_ITEM('Steel','Steel');
#7202=DESCRIPTIVE_REPRESENTATION_ITEM('Steel','Steel');
#7203=DESCRIPTIVE_REPRESENTATION_ITEM('Steel','Steel');
#7204=PROPERTY_DEFINITION('material property','material name',#19677);
#7205=PROPERTY_DEFINITION('material property','density of part',#19677);
#7206=PROPERTY_DEFINITION('material property','material name',#19678);
#7207=PROPERTY_DEFINITION('material property','density of part',#19678);
#7208=PROPERTY_DEFINITION('material property','material name',#19679);
#7209=PROPERTY_DEFINITION('material property','density of part',#19679);
#7210=PROPERTY_DEFINITION('material property','material name',#19680);
#7211=PROPERTY_DEFINITION('material property','density of part',#19680);
#7212=PROPERTY_DEFINITION('material property','material name',#19682);
#7213=PROPERTY_DEFINITION('material property','density of part',#19682);
#7214=PROPERTY_DEFINITION('material property','material name',#19683);
#7215=PROPERTY_DEFINITION('material property','density of part',#19683);
#7216=PROPERTY_DEFINITION('material property','material name',#19684);
#7217=PROPERTY_DEFINITION('material property','density of part',#19684);
#7218=PROPERTY_DEFINITION('material property','material name',#19685);
#7219=PROPERTY_DEFINITION('material property','density of part',#19685);
#7220=PROPERTY_DEFINITION('material property','material name',#19686);
#7221=PROPERTY_DEFINITION('material property','density of part',#19686);
#7222=PROPERTY_DEFINITION('material property','material name',#19687);
#7223=PROPERTY_DEFINITION('material property','density of part',#19687);
#7224=AXIS2_PLACEMENT_3D('',#9318,#7769,#7770);
#7225=AXIS2_PLACEMENT_3D('',#9319,#7771,#7772);
#7226=AXIS2_PLACEMENT_3D('',#9320,#7773,#7774);
#7227=AXIS2_PLACEMENT_3D('',#9322,#7775,#7776);
#7228=AXIS2_PLACEMENT_3D('',#9325,#7778,#7779);
#7229=AXIS2_PLACEMENT_3D('',#9326,#7780,#7781);
#7230=AXIS2_PLACEMENT_3D('',#9328,#7782,#7783);
#7231=AXIS2_PLACEMENT_3D('',#9331,#7785,#7786);
#7232=AXIS2_PLACEMENT_3D('',#9332,#7787,#7788);
#7233=AXIS2_PLACEMENT_3D('',#9334,#7789,#7790);
#7234=AXIS2_PLACEMENT_3D('',#9337,#7792,#7793);
#7235=AXIS2_PLACEMENT_3D('',#9338,#7794,#7795);
#7236=AXIS2_PLACEMENT_3D('',#9345,#7799,#7800);
#7237=AXIS2_PLACEMENT_3D('',#9349,#7802,#7803);
#7238=AXIS2_PLACEMENT_3D('',#9350,#7804,#7805);
#7239=AXIS2_PLACEMENT_3D('',#9351,#7806,#7807);
#7240=AXIS2_PLACEMENT_3D('',#9355,#7810,#7811);
#7241=AXIS2_PLACEMENT_3D('',#9361,#7815,#7816);
#7242=AXIS2_PLACEMENT_3D('',#9370,#7821,#7822);
#7243=AXIS2_PLACEMENT_3D('',#9372,#7823,#7824);
#7244=AXIS2_PLACEMENT_3D('',#9374,#7825,#7826);
#7245=AXIS2_PLACEMENT_3D('',#9376,#7828,#7829);
#7246=AXIS2_PLACEMENT_3D('',#9377,#7830,#7831);
#7247=AXIS2_PLACEMENT_3D('',#9378,#7832,#7833);
#7248=AXIS2_PLACEMENT_3D('',#9379,#7834,#7835);
#7249=AXIS2_PLACEMENT_3D('',#9383,#7838,#7839);
#7250=AXIS2_PLACEMENT_3D('',#9391,#7844,#7845);
#7251=AXIS2_PLACEMENT_3D('',#9397,#7849,#7850);
#7252=AXIS2_PLACEMENT_3D('',#9403,#7854,#7855);
#7253=AXIS2_PLACEMENT_3D('',#9409,#7859,#7860);
#7254=AXIS2_PLACEMENT_3D('',#9411,#7861,#7862);
#7255=AXIS2_PLACEMENT_3D('',#9414,#7864,#7865);
#7256=AXIS2_PLACEMENT_3D('',#9415,#7866,#7867);
#7257=AXIS2_PLACEMENT_3D('',#9417,#7868,#7869);
#7258=AXIS2_PLACEMENT_3D('',#9420,#7871,#7872);
#7259=AXIS2_PLACEMENT_3D('',#9421,#7873,#7874);
#7260=AXIS2_PLACEMENT_3D('',#9425,#7876,#7877);
#7261=AXIS2_PLACEMENT_3D('',#9437,#7883,#7884);
#7262=AXIS2_PLACEMENT_3D('',#9442,#7887,#7888);
#7263=AXIS2_PLACEMENT_3D('',#9443,#7889,#7890);
#7264=AXIS2_PLACEMENT_3D('',#9445,#7891,#7892);
#7265=AXIS2_PLACEMENT_3D('',#9447,#7893,#7894);
#7266=AXIS2_PLACEMENT_3D('',#9448,#7895,#7896);
#7267=AXIS2_PLACEMENT_3D('',#9449,#7897,#7898);
#7268=AXIS2_PLACEMENT_3D('',#9452,#7899,#7900);
#7269=AXIS2_PLACEMENT_3D('',#9453,#7901,#7902);
#7270=AXIS2_PLACEMENT_3D('',#9455,#7904,#7905);
#7271=AXIS2_PLACEMENT_3D('',#9461,#7908,#7909);
#7272=AXIS2_PLACEMENT_3D('',#9473,#7915,#7916);
#7273=AXIS2_PLACEMENT_3D('',#9475,#7918,#7919);
#7274=AXIS2_PLACEMENT_3D('',#9476,#7920,#7921);
#7275=AXIS2_PLACEMENT_3D('',#9477,#7922,#7923);
#7276=AXIS2_PLACEMENT_3D('',#9480,#7926,#7927);
#7277=AXIS2_PLACEMENT_3D('',#9483,#7930,#7931);
#7278=AXIS2_PLACEMENT_3D('',#9485,#7933,#7934);
#7279=AXIS2_PLACEMENT_3D('',#9487,#7936,#7937);
#7280=AXIS2_PLACEMENT_3D('',#9488,#7938,#7939);
#7281=AXIS2_PLACEMENT_3D('',#9490,#7941,#7942);
#7282=AXIS2_PLACEMENT_3D('',#9491,#7943,#7944);
#7283=AXIS2_PLACEMENT_3D('',#9493,#7946,#7947);
#7284=AXIS2_PLACEMENT_3D('',#9495,#7949,#7950);
#7285=AXIS2_PLACEMENT_3D('',#9496,#7951,#7952);
#7286=AXIS2_PLACEMENT_3D('',#9497,#7953,#7954);
#7287=AXIS2_PLACEMENT_3D('',#9499,#7955,#7956);
#7288=AXIS2_PLACEMENT_3D('',#9502,#7958,#7959);
#7289=AXIS2_PLACEMENT_3D('',#9503,#7960,#7961);
#7290=AXIS2_PLACEMENT_3D('',#9505,#7962,#7963);
#7291=AXIS2_PLACEMENT_3D('',#9508,#7965,#7966);
#7292=AXIS2_PLACEMENT_3D('',#9509,#7967,#7968);
#7293=AXIS2_PLACEMENT_3D('',#9511,#7969,#7970);
#7294=AXIS2_PLACEMENT_3D('',#9514,#7972,#7973);
#7295=AXIS2_PLACEMENT_3D('',#9515,#7974,#7975);
#7296=AXIS2_PLACEMENT_3D('',#9524,#7980,#7981);
#7297=AXIS2_PLACEMENT_3D('',#9533,#7986,#7987);
#7298=AXIS2_PLACEMENT_3D('',#9535,#7988,#7989);
#7299=AXIS2_PLACEMENT_3D('',#9537,#7990,#7991);
#7300=AXIS2_PLACEMENT_3D('',#9539,#7993,#7994);
#7301=AXIS2_PLACEMENT_3D('',#9541,#7995,#7996);
#7302=AXIS2_PLACEMENT_3D('',#9543,#7997,#7998);
#7303=AXIS2_PLACEMENT_3D('',#9545,#8000,#8001);
#7304=AXIS2_PLACEMENT_3D('',#9546,#8002,#8003);
#7305=AXIS2_PLACEMENT_3D('',#9547,#8004,#8005);
#7306=AXIS2_PLACEMENT_3D('',#9548,#8006,#8007);
#7307=AXIS2_PLACEMENT_3D('',#9552,#8010,#8011);
#7308=AXIS2_PLACEMENT_3D('',#9560,#8016,#8017);
#7309=AXIS2_PLACEMENT_3D('',#9564,#8020,#8021);
#7310=AXIS2_PLACEMENT_3D('',#9570,#8025,#8026);
#7311=AXIS2_PLACEMENT_3D('',#9576,#8030,#8031);
#7312=AXIS2_PLACEMENT_3D('',#9578,#8032,#8033);
#7313=AXIS2_PLACEMENT_3D('',#9581,#8035,#8036);
#7314=AXIS2_PLACEMENT_3D('',#9582,#8037,#8038);
#7315=AXIS2_PLACEMENT_3D('',#9584,#8039,#8040);
#7316=AXIS2_PLACEMENT_3D('',#9587,#8042,#8043);
#7317=AXIS2_PLACEMENT_3D('',#9588,#8044,#8045);
#7318=AXIS2_PLACEMENT_3D('',#9592,#8047,#8048);
#7319=AXIS2_PLACEMENT_3D('',#9604,#8054,#8055);
#7320=AXIS2_PLACEMENT_3D('',#9609,#8058,#8059);
#7321=AXIS2_PLACEMENT_3D('',#9610,#8060,#8061);
#7322=AXIS2_PLACEMENT_3D('',#9612,#8062,#8063);
#7323=AXIS2_PLACEMENT_3D('',#9614,#8064,#8065);
#7324=AXIS2_PLACEMENT_3D('',#9615,#8066,#8067);
#7325=AXIS2_PLACEMENT_3D('',#9616,#8068,#8069);
#7326=AXIS2_PLACEMENT_3D('',#9619,#8070,#8071);
#7327=AXIS2_PLACEMENT_3D('',#9620,#8072,#8073);
#7328=AXIS2_PLACEMENT_3D('',#9622,#8075,#8076);
#7329=AXIS2_PLACEMENT_3D('',#9628,#8079,#8080);
#7330=AXIS2_PLACEMENT_3D('',#9640,#8086,#8087);
#7331=AXIS2_PLACEMENT_3D('',#9642,#8089,#8090);
#7332=AXIS2_PLACEMENT_3D('',#9643,#8091,#8092);
#7333=AXIS2_PLACEMENT_3D('',#9644,#8093,#8094);
#7334=AXIS2_PLACEMENT_3D('',#9647,#8097,#8098);
#7335=AXIS2_PLACEMENT_3D('',#9650,#8101,#8102);
#7336=AXIS2_PLACEMENT_3D('',#9652,#8104,#8105);
#7337=AXIS2_PLACEMENT_3D('',#9654,#8107,#8108);
#7338=AXIS2_PLACEMENT_3D('',#9655,#8109,#8110);
#7339=AXIS2_PLACEMENT_3D('',#9657,#8112,#8113);
#7340=AXIS2_PLACEMENT_3D('',#9658,#8114,#8115);
#7341=AXIS2_PLACEMENT_3D('',#9660,#8117,#8118);
#7342=AXIS2_PLACEMENT_3D('',#9662,#8120,#8121);
#7343=AXIS2_PLACEMENT_3D('',#9663,#8122,#8123);
#7344=AXIS2_PLACEMENT_3D('',#9664,#8124,#8125);
#7345=AXIS2_PLACEMENT_3D('',#9666,#8126,#8127);
#7346=AXIS2_PLACEMENT_3D('',#9669,#8129,#8130);
#7347=AXIS2_PLACEMENT_3D('',#9670,#8131,#8132);
#7348=AXIS2_PLACEMENT_3D('',#9672,#8133,#8134);
#7349=AXIS2_PLACEMENT_3D('',#9673,#8135,#8136);
#7350=AXIS2_PLACEMENT_3D('',#9675,#8137,#8138);
#7351=AXIS2_PLACEMENT_3D('',#9676,#8139,#8140);
#7352=AXIS2_PLACEMENT_3D('',#9678,#8141,#8142);
#7353=AXIS2_PLACEMENT_3D('',#9680,#8144,#8145);
#7354=AXIS2_PLACEMENT_3D('',#9682,#8146,#8147);
#7355=AXIS2_PLACEMENT_3D('',#9684,#8148,#8149);
#7356=AXIS2_PLACEMENT_3D('',#9685,#8150,#8151);
#7357=AXIS2_PLACEMENT_3D('',#9688,#8153,#8154);
#7358=AXIS2_PLACEMENT_3D('',#9689,#8155,#8156);
#7359=AXIS2_PLACEMENT_3D('',#9690,#8157,#8158);
#7360=AXIS2_PLACEMENT_3D('',#9692,#8160,#8161);
#7361=AXIS2_PLACEMENT_3D('',#9693,#8162,#8163);
#7362=AXIS2_PLACEMENT_3D('',#9694,#8164,#8165);
#7363=AXIS2_PLACEMENT_3D('',#9703,#8170,#8171);
#7364=AXIS2_PLACEMENT_3D('',#9712,#8176,#8177);
#7365=AXIS2_PLACEMENT_3D('',#9713,#8178,#8179);
#7366=AXIS2_PLACEMENT_3D('',#9714,#8180,#8181);
#7367=AXIS2_PLACEMENT_3D('',#9715,#8182,#8183);
#7368=AXIS2_PLACEMENT_3D('',#9716,#8184,#8185);
#7369=AXIS2_PLACEMENT_3D('',#9717,#8186,#8187);
#7370=AXIS2_PLACEMENT_3D('',#9718,#8188,#8189);
#7371=AXIS2_PLACEMENT_3D('',#9719,#8190,#8191);
#7372=AXIS2_PLACEMENT_3D('',#9720,#8192,#8193);
#7373=AXIS2_PLACEMENT_3D('',#9721,#8194,#8195);
#7374=AXIS2_PLACEMENT_3D('',#9722,#8196,#8197);
#7375=AXIS2_PLACEMENT_3D('',#9788,#8200,#8201);
#7376=AXIS2_PLACEMENT_3D('',#9790,#8202,#8203);
#7377=AXIS2_PLACEMENT_3D('',#9792,#8204,#8205);
#7378=AXIS2_PLACEMENT_3D('',#9793,#8206,#8207);
#7379=AXIS2_PLACEMENT_3D('',#9795,#8208,#8209);
#7380=AXIS2_PLACEMENT_3D('',#9798,#8211,#8212);
#7381=AXIS2_PLACEMENT_3D('',#9799,#8213,#8214);
#7382=AXIS2_PLACEMENT_3D('',#9801,#8215,#8216);
#7383=AXIS2_PLACEMENT_3D('',#9803,#8218,#8219);
#7384=AXIS2_PLACEMENT_3D('',#9805,#8220,#8221);
#7385=AXIS2_PLACEMENT_3D('',#9807,#8223,#8224);
#7386=AXIS2_PLACEMENT_3D('',#9809,#8225,#8226);
#7387=AXIS2_PLACEMENT_3D('',#9812,#8228,#8229);
#7388=AXIS2_PLACEMENT_3D('',#9813,#8230,#8231);
#7389=AXIS2_PLACEMENT_3D('',#9815,#8232,#8233);
#7390=AXIS2_PLACEMENT_3D('',#9818,#8235,#8236);
#7391=AXIS2_PLACEMENT_3D('',#9819,#8237,#8238);
#7392=AXIS2_PLACEMENT_3D('',#9821,#8239,#8240);
#7393=AXIS2_PLACEMENT_3D('',#9822,#8241,#8242);
#7394=AXIS2_PLACEMENT_3D('',#9824,#8243,#8244);
#7395=AXIS2_PLACEMENT_3D('',#9827,#8246,#8247);
#7396=AXIS2_PLACEMENT_3D('',#9828,#8248,#8249);
#7397=AXIS2_PLACEMENT_3D('',#9830,#8250,#8251);
#7398=AXIS2_PLACEMENT_3D('',#9831,#8252,#8253);
#7399=AXIS2_PLACEMENT_3D('',#9834,#8255,#8256);
#7400=AXIS2_PLACEMENT_3D('',#9835,#8257,#8258);
#7401=AXIS2_PLACEMENT_3D('',#9838,#8260,#8261);
#7402=AXIS2_PLACEMENT_3D('',#9839,#8262,#8263);
#7403=AXIS2_PLACEMENT_3D('',#9848,#8268,#8269);
#7404=AXIS2_PLACEMENT_3D('',#9857,#8274,#8275);
#7405=AXIS2_PLACEMENT_3D('',#9866,#8280,#8281);
#7406=AXIS2_PLACEMENT_3D('',#9875,#8286,#8287);
#7407=AXIS2_PLACEMENT_3D('',#9884,#8292,#8293);
#7408=AXIS2_PLACEMENT_3D('',#9893,#8298,#8299);
#7409=AXIS2_PLACEMENT_3D('',#9902,#8304,#8305);
#7410=AXIS2_PLACEMENT_3D('',#9904,#8306,#8307);
#7411=AXIS2_PLACEMENT_3D('',#9905,#8308,#8309);
#7412=AXIS2_PLACEMENT_3D('',#9907,#8310,#8311);
#7413=AXIS2_PLACEMENT_3D('',#9908,#8312,#8313);
#7414=AXIS2_PLACEMENT_3D('',#9911,#8316,#8317);
#7415=AXIS2_PLACEMENT_3D('',#9914,#8320,#8321);
#7416=AXIS2_PLACEMENT_3D('',#9917,#8324,#8325);
#7417=AXIS2_PLACEMENT_3D('',#9923,#8329,#8330);
#7418=AXIS2_PLACEMENT_3D('',#9929,#8334,#8335);
#7419=AXIS2_PLACEMENT_3D('',#10006,#8338,#8339);
#7420=AXIS2_PLACEMENT_3D('',#10084,#8343,#8344);
#7421=AXIS2_PLACEMENT_3D('',#10162,#8348,#8349);
#7422=AXIS2_PLACEMENT_3D('',#10237,#8352,#8353);
#7423=AXIS2_PLACEMENT_3D('',#10253,#8357,#8358);
#7424=AXIS2_PLACEMENT_3D('',#10631,#8370,#8371);
#7425=AXIS2_PLACEMENT_3D('',#10633,#8372,#8373);
#7426=AXIS2_PLACEMENT_3D('',#10635,#8375,#8376);
#7427=AXIS2_PLACEMENT_3D('',#10637,#8378,#8379);
#7428=AXIS2_PLACEMENT_3D('',#10805,#8381,#8382);
#7429=AXIS2_PLACEMENT_3D('',#10806,#8383,#8384);
#7430=AXIS2_PLACEMENT_3D('',#10811,#8385,#8386);
#7431=AXIS2_PLACEMENT_3D('',#10883,#8388,#8389);
#7432=AXIS2_PLACEMENT_3D('',#11001,#8391,#8392);
#7433=AXIS2_PLACEMENT_3D('',#11046,#8393,#8394);
#7434=AXIS2_PLACEMENT_3D('',#11197,#8395,#8396);
#7435=AXIS2_PLACEMENT_3D('',#11317,#8398,#8399);
#7436=AXIS2_PLACEMENT_3D('',#11322,#8400,#8401);
#7437=AXIS2_PLACEMENT_3D('',#11374,#8403,#8404);
#7438=AXIS2_PLACEMENT_3D('',#11375,#8405,#8406);
#7439=AXIS2_PLACEMENT_3D('',#11376,#8407,#8408);
#7440=AXIS2_PLACEMENT_3D('',#11377,#8409,#8410);
#7441=AXIS2_PLACEMENT_3D('',#11378,#8411,#8412);
#7442=AXIS2_PLACEMENT_3D('',#11379,#8413,#8414);
#7443=AXIS2_PLACEMENT_3D('',#11381,#8415,#8416);
#7444=AXIS2_PLACEMENT_3D('',#11382,#8417,#8418);
#7445=AXIS2_PLACEMENT_3D('',#11383,#8419,#8420);
#7446=AXIS2_PLACEMENT_3D('',#11384,#8421,#8422);
#7447=AXIS2_PLACEMENT_3D('',#11385,#8423,#8424);
#7448=AXIS2_PLACEMENT_3D('',#11386,#8425,#8426);
#7449=AXIS2_PLACEMENT_3D('',#11407,#8427,#8428);
#7450=AXIS2_PLACEMENT_3D('',#11409,#8429,#8430);
#7451=AXIS2_PLACEMENT_3D('',#11410,#8431,#8432);
#7452=AXIS2_PLACEMENT_3D('',#11411,#8433,#8434);
#7453=AXIS2_PLACEMENT_3D('',#11509,#8436,#8437);
#7454=AXIS2_PLACEMENT_3D('',#11510,#8438,#8439);
#7455=AXIS2_PLACEMENT_3D('',#11513,#8440,#8441);
#7456=AXIS2_PLACEMENT_3D('',#11515,#8442,#8443);
#7457=AXIS2_PLACEMENT_3D('',#11516,#8444,#8445);
#7458=AXIS2_PLACEMENT_3D('',#11517,#8446,#8447);
#7459=AXIS2_PLACEMENT_3D('',#11520,#8448,#8449);
#7460=AXIS2_PLACEMENT_3D('',#11522,#8450,#8451);
#7461=AXIS2_PLACEMENT_3D('',#11523,#8452,#8453);
#7462=AXIS2_PLACEMENT_3D('',#11524,#8454,#8455);
#7463=AXIS2_PLACEMENT_3D('',#11527,#8456,#8457);
#7464=AXIS2_PLACEMENT_3D('',#11529,#8458,#8459);
#7465=AXIS2_PLACEMENT_3D('',#11530,#8460,#8461);
#7466=AXIS2_PLACEMENT_3D('',#11531,#8462,#8463);
#7467=AXIS2_PLACEMENT_3D('',#11562,#8466,#8467);
#7468=AXIS2_PLACEMENT_3D('',#11565,#8468,#8469);
#7469=AXIS2_PLACEMENT_3D('',#11567,#8470,#8471);
#7470=AXIS2_PLACEMENT_3D('',#11568,#8472,#8473);
#7471=AXIS2_PLACEMENT_3D('',#11569,#8474,#8475);
#7472=AXIS2_PLACEMENT_3D('',#11750,#8478,#8479);
#7473=AXIS2_PLACEMENT_3D('',#11751,#8480,#8481);
#7474=AXIS2_PLACEMENT_3D('',#11768,#8482,#8483);
#7475=AXIS2_PLACEMENT_3D('',#11769,#8484,#8485);
#7476=AXIS2_PLACEMENT_3D('',#11770,#8486,#8487);
#7477=AXIS2_PLACEMENT_3D('',#11836,#8490,#8491);
#7478=AXIS2_PLACEMENT_3D('',#11838,#8492,#8493);
#7479=AXIS2_PLACEMENT_3D('',#11840,#8494,#8495);
#7480=AXIS2_PLACEMENT_3D('',#11841,#8496,#8497);
#7481=AXIS2_PLACEMENT_3D('',#11843,#8498,#8499);
#7482=AXIS2_PLACEMENT_3D('',#11846,#8501,#8502);
#7483=AXIS2_PLACEMENT_3D('',#11847,#8503,#8504);
#7484=AXIS2_PLACEMENT_3D('',#11849,#8505,#8506);
#7485=AXIS2_PLACEMENT_3D('',#11851,#8508,#8509);
#7486=AXIS2_PLACEMENT_3D('',#11853,#8510,#8511);
#7487=AXIS2_PLACEMENT_3D('',#11855,#8513,#8514);
#7488=AXIS2_PLACEMENT_3D('',#11857,#8515,#8516);
#7489=AXIS2_PLACEMENT_3D('',#11860,#8518,#8519);
#7490=AXIS2_PLACEMENT_3D('',#11861,#8520,#8521);
#7491=AXIS2_PLACEMENT_3D('',#11870,#8526,#8527);
#7492=AXIS2_PLACEMENT_3D('',#11876,#8531,#8532);
#7493=AXIS2_PLACEMENT_3D('',#11882,#8536,#8537);
#7494=AXIS2_PLACEMENT_3D('',#11888,#8541,#8542);
#7495=AXIS2_PLACEMENT_3D('',#11894,#8546,#8547);
#7496=AXIS2_PLACEMENT_3D('',#11897,#8550,#8551);
#7497=AXIS2_PLACEMENT_3D('',#11899,#8552,#8553);
#7498=AXIS2_PLACEMENT_3D('',#11900,#8554,#8555);
#7499=AXIS2_PLACEMENT_3D('',#11909,#8560,#8561);
#7500=AXIS2_PLACEMENT_3D('',#11915,#8565,#8566);
#7501=AXIS2_PLACEMENT_3D('',#11921,#8570,#8571);
#7502=AXIS2_PLACEMENT_3D('',#11927,#8575,#8576);
#7503=AXIS2_PLACEMENT_3D('',#11933,#8580,#8581);
#7504=AXIS2_PLACEMENT_3D('',#11936,#8584,#8585);
#7505=AXIS2_PLACEMENT_3D('',#11938,#8586,#8587);
#7506=AXIS2_PLACEMENT_3D('',#11939,#8588,#8589);
#7507=AXIS2_PLACEMENT_3D('',#11942,#8591,#8592);
#7508=AXIS2_PLACEMENT_3D('',#11943,#8593,#8594);
#7509=AXIS2_PLACEMENT_3D('',#11946,#8596,#8597);
#7510=AXIS2_PLACEMENT_3D('',#11947,#8598,#8599);
#7511=AXIS2_PLACEMENT_3D('',#11956,#8604,#8605);
#7512=AXIS2_PLACEMENT_3D('',#11965,#8610,#8611);
#7513=AXIS2_PLACEMENT_3D('',#11974,#8616,#8617);
#7514=AXIS2_PLACEMENT_3D('',#11983,#8622,#8623);
#7515=AXIS2_PLACEMENT_3D('',#11992,#8628,#8629);
#7516=AXIS2_PLACEMENT_3D('',#12001,#8634,#8635);
#7517=AXIS2_PLACEMENT_3D('',#12010,#8640,#8641);
#7518=AXIS2_PLACEMENT_3D('',#12012,#8642,#8643);
#7519=AXIS2_PLACEMENT_3D('',#12013,#8644,#8645);
#7520=AXIS2_PLACEMENT_3D('',#12015,#8646,#8647);
#7521=AXIS2_PLACEMENT_3D('',#12016,#8648,#8649);
#7522=AXIS2_PLACEMENT_3D('',#12019,#8652,#8653);
#7523=AXIS2_PLACEMENT_3D('',#12022,#8656,#8657);
#7524=AXIS2_PLACEMENT_3D('',#12025,#8660,#8661);
#7525=AXIS2_PLACEMENT_3D('',#12031,#8665,#8666);
#7526=AXIS2_PLACEMENT_3D('',#12037,#8670,#8671);
#7527=AXIS2_PLACEMENT_3D('',#12114,#8674,#8675);
#7528=AXIS2_PLACEMENT_3D('',#12192,#8679,#8680);
#7529=AXIS2_PLACEMENT_3D('',#12270,#8684,#8685);
#7530=AXIS2_PLACEMENT_3D('',#12345,#8688,#8689);
#7531=AXIS2_PLACEMENT_3D('',#12361,#8693,#8694);
#7532=AXIS2_PLACEMENT_3D('',#12739,#8706,#8707);
#7533=AXIS2_PLACEMENT_3D('',#12741,#8708,#8709);
#7534=AXIS2_PLACEMENT_3D('',#12743,#8711,#8712);
#7535=AXIS2_PLACEMENT_3D('',#12745,#8714,#8715);
#7536=AXIS2_PLACEMENT_3D('',#12913,#8717,#8718);
#7537=AXIS2_PLACEMENT_3D('',#12914,#8719,#8720);
#7538=AXIS2_PLACEMENT_3D('',#12919,#8721,#8722);
#7539=AXIS2_PLACEMENT_3D('',#12991,#8724,#8725);
#7540=AXIS2_PLACEMENT_3D('',#13109,#8727,#8728);
#7541=AXIS2_PLACEMENT_3D('',#13154,#8729,#8730);
#7542=AXIS2_PLACEMENT_3D('',#13305,#8731,#8732);
#7543=AXIS2_PLACEMENT_3D('',#13425,#8734,#8735);
#7544=AXIS2_PLACEMENT_3D('',#13430,#8736,#8737);
#7545=AXIS2_PLACEMENT_3D('',#13482,#8739,#8740);
#7546=AXIS2_PLACEMENT_3D('',#13483,#8741,#8742);
#7547=AXIS2_PLACEMENT_3D('',#13484,#8743,#8744);
#7548=AXIS2_PLACEMENT_3D('',#13485,#8745,#8746);
#7549=AXIS2_PLACEMENT_3D('',#13486,#8747,#8748);
#7550=AXIS2_PLACEMENT_3D('',#13487,#8749,#8750);
#7551=AXIS2_PLACEMENT_3D('',#13489,#8751,#8752);
#7552=AXIS2_PLACEMENT_3D('',#13490,#8753,#8754);
#7553=AXIS2_PLACEMENT_3D('',#13491,#8755,#8756);
#7554=AXIS2_PLACEMENT_3D('',#13492,#8757,#8758);
#7555=AXIS2_PLACEMENT_3D('',#13493,#8759,#8760);
#7556=AXIS2_PLACEMENT_3D('',#13494,#8761,#8762);
#7557=AXIS2_PLACEMENT_3D('',#13515,#8763,#8764);
#7558=AXIS2_PLACEMENT_3D('',#13517,#8765,#8766);
#7559=AXIS2_PLACEMENT_3D('',#13518,#8767,#8768);
#7560=AXIS2_PLACEMENT_3D('',#13519,#8769,#8770);
#7561=AXIS2_PLACEMENT_3D('',#13617,#8772,#8773);
#7562=AXIS2_PLACEMENT_3D('',#13618,#8774,#8775);
#7563=AXIS2_PLACEMENT_3D('',#13621,#8776,#8777);
#7564=AXIS2_PLACEMENT_3D('',#13623,#8778,#8779);
#7565=AXIS2_PLACEMENT_3D('',#13624,#8780,#8781);
#7566=AXIS2_PLACEMENT_3D('',#13625,#8782,#8783);
#7567=AXIS2_PLACEMENT_3D('',#13628,#8784,#8785);
#7568=AXIS2_PLACEMENT_3D('',#13630,#8786,#8787);
#7569=AXIS2_PLACEMENT_3D('',#13631,#8788,#8789);
#7570=AXIS2_PLACEMENT_3D('',#13632,#8790,#8791);
#7571=AXIS2_PLACEMENT_3D('',#13635,#8792,#8793);
#7572=AXIS2_PLACEMENT_3D('',#13637,#8794,#8795);
#7573=AXIS2_PLACEMENT_3D('',#13638,#8796,#8797);
#7574=AXIS2_PLACEMENT_3D('',#13639,#8798,#8799);
#7575=AXIS2_PLACEMENT_3D('',#13670,#8802,#8803);
#7576=AXIS2_PLACEMENT_3D('',#13673,#8804,#8805);
#7577=AXIS2_PLACEMENT_3D('',#13675,#8806,#8807);
#7578=AXIS2_PLACEMENT_3D('',#13676,#8808,#8809);
#7579=AXIS2_PLACEMENT_3D('',#13677,#8810,#8811);
#7580=AXIS2_PLACEMENT_3D('',#13858,#8814,#8815);
#7581=AXIS2_PLACEMENT_3D('',#13859,#8816,#8817);
#7582=AXIS2_PLACEMENT_3D('',#13876,#8818,#8819);
#7583=AXIS2_PLACEMENT_3D('',#13877,#8820,#8821);
#7584=AXIS2_PLACEMENT_3D('',#13878,#8822,#8823);
#7585=AXIS2_PLACEMENT_3D('',#13880,#8824,#8825);
#7586=AXIS2_PLACEMENT_3D('',#13883,#8827,#8828);
#7587=AXIS2_PLACEMENT_3D('',#13884,#8829,#8830);
#7588=AXIS2_PLACEMENT_3D('',#13886,#8831,#8832);
#7589=AXIS2_PLACEMENT_3D('',#13889,#8834,#8835);
#7590=AXIS2_PLACEMENT_3D('',#13890,#8836,#8837);
#7591=AXIS2_PLACEMENT_3D('',#13892,#8838,#8839);
#7592=AXIS2_PLACEMENT_3D('',#13894,#8840,#8841);
#7593=AXIS2_PLACEMENT_3D('',#13895,#8842,#8843);
#7594=AXIS2_PLACEMENT_3D('',#13897,#8844,#8845);
#7595=AXIS2_PLACEMENT_3D('',#13899,#8847,#8848);
#7596=AXIS2_PLACEMENT_3D('',#13900,#8849,#8850);
#7597=AXIS2_PLACEMENT_3D('',#13902,#8851,#8852);
#7598=AXIS2_PLACEMENT_3D('',#13904,#8853,#8854);
#7599=AXIS2_PLACEMENT_3D('',#13905,#8855,#8856);
#7600=AXIS2_PLACEMENT_3D('',#13907,#8857,#8858);
#7601=AXIS2_PLACEMENT_3D('',#13909,#8860,#8861);
#7602=AXIS2_PLACEMENT_3D('',#13910,#8862,#8863);
#7603=AXIS2_PLACEMENT_3D('',#13912,#8864,#8865);
#7604=AXIS2_PLACEMENT_3D('',#13914,#8866,#8867);
#7605=AXIS2_PLACEMENT_3D('',#13915,#8868,#8869);
#7606=AXIS2_PLACEMENT_3D('',#13917,#8870,#8871);
#7607=AXIS2_PLACEMENT_3D('',#13919,#8873,#8874);
#7608=AXIS2_PLACEMENT_3D('',#13920,#8875,#8876);
#7609=AXIS2_PLACEMENT_3D('',#13922,#8877,#8878);
#7610=AXIS2_PLACEMENT_3D('',#13924,#8879,#8880);
#7611=AXIS2_PLACEMENT_3D('',#13925,#8881,#8882);
#7612=AXIS2_PLACEMENT_3D('',#13927,#8883,#8884);
#7613=AXIS2_PLACEMENT_3D('',#13929,#8886,#8887);
#7614=AXIS2_PLACEMENT_3D('',#13930,#8888,#8889);
#7615=AXIS2_PLACEMENT_3D('',#13933,#8891,#8892);
#7616=AXIS2_PLACEMENT_3D('',#13934,#8893,#8894);
#7617=AXIS2_PLACEMENT_3D('',#13937,#8896,#8897);
#7618=AXIS2_PLACEMENT_3D('',#13938,#8898,#8899);
#7619=AXIS2_PLACEMENT_3D('',#13941,#8901,#8902);
#7620=AXIS2_PLACEMENT_3D('',#13942,#8903,#8904);
#7621=AXIS2_PLACEMENT_3D('',#13945,#8906,#8907);
#7622=AXIS2_PLACEMENT_3D('',#13973,#8908,#8909);
#7623=AXIS2_PLACEMENT_3D('',#13981,#8910,#8911);
#7624=AXIS2_PLACEMENT_3D('',#13987,#8912,#8913);
#7625=AXIS2_PLACEMENT_3D('',#13990,#8914,#8915);
#7626=AXIS2_PLACEMENT_3D('',#14020,#8918,#8919);
#7627=AXIS2_PLACEMENT_3D('',#14058,#8920,#8921);
#7628=AXIS2_PLACEMENT_3D('',#14096,#8922,#8923);
#7629=AXIS2_PLACEMENT_3D('',#14107,#8924,#8925);
#7630=AXIS2_PLACEMENT_3D('',#14110,#8926,#8927);
#7631=AXIS2_PLACEMENT_3D('',#14140,#8930,#8931);
#7632=AXIS2_PLACEMENT_3D('',#14186,#8932,#8933);
#7633=AXIS2_PLACEMENT_3D('',#14339,#8935,#8936);
#7634=AXIS2_PLACEMENT_3D('',#14340,#8937,#8938);
#7635=AXIS2_PLACEMENT_3D('',#14463,#8940,#8941);
#7636=AXIS2_PLACEMENT_3D('',#14484,#8942,#8943);
#7637=AXIS2_PLACEMENT_3D('',#14485,#8944,#8945);
#7638=AXIS2_PLACEMENT_3D('',#14501,#8947,#8948);
#7639=AXIS2_PLACEMENT_3D('',#14509,#8949,#8950);
#7640=AXIS2_PLACEMENT_3D('',#14557,#8952,#8953);
#7641=AXIS2_PLACEMENT_3D('',#14605,#8955,#8956);
#7642=AXIS2_PLACEMENT_3D('',#14656,#8958,#8959);
#7643=AXIS2_PLACEMENT_3D('',#14704,#8961,#8962);
#7644=AXIS2_PLACEMENT_3D('',#14752,#8964,#8965);
#7645=AXIS2_PLACEMENT_3D('',#14800,#8967,#8968);
#7646=AXIS2_PLACEMENT_3D('',#14854,#8970,#8971);
#7647=AXIS2_PLACEMENT_3D('',#14902,#8973,#8974);
#7648=AXIS2_PLACEMENT_3D('',#14950,#8976,#8977);
#7649=AXIS2_PLACEMENT_3D('',#15004,#8979,#8980);
#7650=AXIS2_PLACEMENT_3D('',#15052,#8982,#8983);
#7651=AXIS2_PLACEMENT_3D('',#15100,#8985,#8986);
#7652=AXIS2_PLACEMENT_3D('',#15148,#8988,#8989);
#7653=AXIS2_PLACEMENT_3D('',#15202,#8991,#8992);
#7654=AXIS2_PLACEMENT_3D('',#15250,#8994,#8995);
#7655=AXIS2_PLACEMENT_3D('',#15298,#8997,#8998);
#7656=AXIS2_PLACEMENT_3D('',#15352,#9000,#9001);
#7657=AXIS2_PLACEMENT_3D('',#15400,#9003,#9004);
#7658=AXIS2_PLACEMENT_3D('',#15448,#9006,#9007);
#7659=AXIS2_PLACEMENT_3D('',#15502,#9009,#9010);
#7660=AXIS2_PLACEMENT_3D('',#15550,#9012,#9013);
#7661=AXIS2_PLACEMENT_3D('',#15598,#9015,#9016);
#7662=AXIS2_PLACEMENT_3D('',#15646,#9018,#9019);
#7663=AXIS2_PLACEMENT_3D('',#15700,#9021,#9022);
#7664=AXIS2_PLACEMENT_3D('',#15748,#9024,#9025);
#7665=AXIS2_PLACEMENT_3D('',#15796,#9027,#9028);
#7666=AXIS2_PLACEMENT_3D('',#15850,#9030,#9031);
#7667=AXIS2_PLACEMENT_3D('',#15898,#9033,#9034);
#7668=AXIS2_PLACEMENT_3D('',#15946,#9036,#9037);
#7669=AXIS2_PLACEMENT_3D('',#15962,#9039,#9040);
#7670=AXIS2_PLACEMENT_3D('',#15972,#9041,#9042);
#7671=AXIS2_PLACEMENT_3D('',#15996,#9044,#9045);
#7672=AXIS2_PLACEMENT_3D('',#16020,#9047,#9048);
#7673=AXIS2_PLACEMENT_3D('',#16045,#9050,#9051);
#7674=AXIS2_PLACEMENT_3D('',#16070,#9053,#9054);
#7675=AXIS2_PLACEMENT_3D('',#16094,#9056,#9057);
#7676=AXIS2_PLACEMENT_3D('',#16119,#9059,#9060);
#7677=AXIS2_PLACEMENT_3D('',#16144,#9062,#9063);
#7678=AXIS2_PLACEMENT_3D('',#16168,#9065,#9066);
#7679=AXIS2_PLACEMENT_3D('',#16192,#9068,#9069);
#7680=AXIS2_PLACEMENT_3D('',#16217,#9071,#9072);
#7681=AXIS2_PLACEMENT_3D('',#16242,#9074,#9075);
#7682=AXIS2_PLACEMENT_3D('',#16266,#9077,#9078);
#7683=AXIS2_PLACEMENT_3D('',#16291,#9080,#9081);
#7684=AXIS2_PLACEMENT_3D('',#16316,#9083,#9084);
#7685=AXIS2_PLACEMENT_3D('',#16340,#9086,#9087);
#7686=AXIS2_PLACEMENT_3D('',#16365,#9089,#9090);
#7687=AXIS2_PLACEMENT_3D('',#16390,#9092,#9093);
#7688=AXIS2_PLACEMENT_3D('',#16414,#9095,#9096);
#7689=AXIS2_PLACEMENT_3D('',#16438,#9098,#9099);
#7690=AXIS2_PLACEMENT_3D('',#16463,#9101,#9102);
#7691=AXIS2_PLACEMENT_3D('',#16488,#9104,#9105);
#7692=AXIS2_PLACEMENT_3D('',#16512,#9107,#9108);
#7693=AXIS2_PLACEMENT_3D('',#16537,#9110,#9111);
#7694=AXIS2_PLACEMENT_3D('',#16562,#9113,#9114);
#7695=AXIS2_PLACEMENT_3D('',#16586,#9116,#9117);
#7696=AXIS2_PLACEMENT_3D('',#16611,#9119,#9120);
#7697=AXIS2_PLACEMENT_3D('',#16635,#9122,#9123);
#7698=AXIS2_PLACEMENT_3D('',#16660,#9125,#9126);
#7699=AXIS2_PLACEMENT_3D('',#16684,#9128,#9129);
#7700=AXIS2_PLACEMENT_3D('',#16846,#9130,#9131);
#7701=AXIS2_PLACEMENT_3D('',#16865,#9133,#9134);
#7702=AXIS2_PLACEMENT_3D('',#17727,#9135,#9136);
#7703=AXIS2_PLACEMENT_3D('',#17738,#9137,#9138);
#7704=AXIS2_PLACEMENT_3D('',#18605,#9139,#9140);
#7705=AXIS2_PLACEMENT_3D('',#18606,#9141,#9142);
#7706=AXIS2_PLACEMENT_3D('',#18615,#9147,#9148);
#7707=AXIS2_PLACEMENT_3D('',#18621,#9152,#9153);
#7708=AXIS2_PLACEMENT_3D('',#18627,#9157,#9158);
#7709=AXIS2_PLACEMENT_3D('',#18633,#9162,#9163);
#7710=AXIS2_PLACEMENT_3D('',#18639,#9167,#9168);
#7711=AXIS2_PLACEMENT_3D('',#18642,#9171,#9172);
#7712=AXIS2_PLACEMENT_3D('',#18643,#9173,#9174);
#7713=AXIS2_PLACEMENT_3D('',#18645,#9175,#9176);
#7714=AXIS2_PLACEMENT_3D('',#18646,#9177,#9178);
#7715=AXIS2_PLACEMENT_3D('',#18649,#9180,#9181);
#7716=AXIS2_PLACEMENT_3D('',#18650,#9182,#9183);
#7717=AXIS2_PLACEMENT_3D('',#18651,#9184,#9185);
#7718=AXIS2_PLACEMENT_3D('',#18652,#9186,#9187);
#7719=AXIS2_PLACEMENT_3D('',#18653,#9188,#9189);
#7720=AXIS2_PLACEMENT_3D('',#18658,#9191,#9192);
#7721=AXIS2_PLACEMENT_3D('',#18666,#9193,#9194);
#7722=AXIS2_PLACEMENT_3D('',#18690,#9196,#9197);
#7723=AXIS2_PLACEMENT_3D('',#18713,#9198,#9199);
#7724=AXIS2_PLACEMENT_3D('',#18767,#9201,#9202);
#7725=AXIS2_PLACEMENT_3D('',#18815,#9204,#9205);
#7726=AXIS2_PLACEMENT_3D('',#18834,#9207,#9208);
#7727=AXIS2_PLACEMENT_3D('',#18854,#9209,#9210);
#7728=AXIS2_PLACEMENT_3D('',#18867,#9212,#9213);
#7729=AXIS2_PLACEMENT_3D('',#18875,#9214,#9215);
#7730=AXIS2_PLACEMENT_3D('',#18900,#9217,#9218);
#7731=AXIS2_PLACEMENT_3D('',#18925,#9220,#9221);
#7732=AXIS2_PLACEMENT_3D('',#18950,#9223,#9224);
#7733=AXIS2_PLACEMENT_3D('',#18961,#9226,#9227);
#7734=AXIS2_PLACEMENT_3D('',#18967,#9228,#9229);
#7735=AXIS2_PLACEMENT_3D('',#19523,#9230,#9231);
#7736=AXIS2_PLACEMENT_3D('',#19536,#9238,#9239);
#7737=AXIS2_PLACEMENT_3D('',#19537,#9240,#9241);
#7738=AXIS2_PLACEMENT_3D('',#19543,#9245,#9246);
#7739=AXIS2_PLACEMENT_3D('',#19547,#9249,#9250);
#7740=AXIS2_PLACEMENT_3D('',#19551,#9253,#9254);
#7741=AXIS2_PLACEMENT_3D('',#19555,#9257,#9258);
#7742=AXIS2_PLACEMENT_3D('',#19559,#9261,#9262);
#7743=AXIS2_PLACEMENT_3D('',#19561,#9264,#9265);
#7744=AXIS2_PLACEMENT_3D('',#19562,#9266,#9267);
#7745=AXIS2_PLACEMENT_3D('',#19563,#9268,#9269);
#7746=AXIS2_PLACEMENT_3D('',#19564,#9270,#9271);
#7747=AXIS2_PLACEMENT_3D('',#19565,#9272,#9273);
#7748=AXIS2_PLACEMENT_3D('',#19566,#9274,#9275);
#7749=AXIS2_PLACEMENT_3D('',#19567,#9276,#9277);
#7750=AXIS2_PLACEMENT_3D('',#19568,#9278,#9279);
#7751=AXIS2_PLACEMENT_3D('',#19569,#9280,#9281);
#7752=AXIS2_PLACEMENT_3D('',#19570,#9282,#9283);
#7753=AXIS2_PLACEMENT_3D('',#19571,#9284,#9285);
#7754=AXIS2_PLACEMENT_3D('',#19573,#9286,#9287);
#7755=AXIS2_PLACEMENT_3D('',#19576,#9289,#9290);
#7756=AXIS2_PLACEMENT_3D('',#19577,#9291,#9292);
#7757=AXIS2_PLACEMENT_3D('',#19579,#9293,#9294);
#7758=AXIS2_PLACEMENT_3D('',#19582,#9296,#9297);
#7759=AXIS2_PLACEMENT_3D('',#19583,#9298,#9299);
#7760=AXIS2_PLACEMENT_3D('',#19584,#9300,#9301);
#7761=AXIS2_PLACEMENT_3D('',#19585,#9302,#9303);
#7762=AXIS2_PLACEMENT_3D('',#19586,#9304,#9305);
#7763=AXIS2_PLACEMENT_3D('',#19587,#9306,#9307);
#7764=AXIS2_PLACEMENT_3D('',#19588,#9308,#9309);
#7765=AXIS2_PLACEMENT_3D('',#19589,#9310,#9311);
#7766=AXIS2_PLACEMENT_3D('',#19590,#9312,#9313);
#7767=AXIS2_PLACEMENT_3D('',#19591,#9314,#9315);
#7768=AXIS2_PLACEMENT_3D('',#19592,#9316,#9317);
#7769=DIRECTION('axis',(0.,0.,1.));
#7770=DIRECTION('refdir',(1.,0.,0.));
#7771=DIRECTION('axis',(0.,0.,1.));
#7772=DIRECTION('refdir',(1.,0.,0.));
#7773=DIRECTION('center_axis',(0.,0.,-1.));
#7774=DIRECTION('ref_axis',(1.,0.,0.));
#7775=DIRECTION('center_axis',(0.,0.,-1.));
#7776=DIRECTION('ref_axis',(1.,0.,0.));
#7777=DIRECTION('',(0.,0.,-1.));
#7778=DIRECTION('center_axis',(0.,0.,1.));
#7779=DIRECTION('ref_axis',(1.,0.,0.));
#7780=DIRECTION('center_axis',(0.,0.,-1.));
#7781=DIRECTION('ref_axis',(1.,0.,0.));
#7782=DIRECTION('center_axis',(0.,0.,-1.));
#7783=DIRECTION('ref_axis',(1.,0.,0.));
#7784=DIRECTION('',(0.,0.,-1.));
#7785=DIRECTION('center_axis',(0.,0.,1.));
#7786=DIRECTION('ref_axis',(1.,0.,0.));
#7787=DIRECTION('center_axis',(0.,0.,-1.));
#7788=DIRECTION('ref_axis',(1.,0.,0.));
#7789=DIRECTION('center_axis',(0.,0.,-1.));
#7790=DIRECTION('ref_axis',(1.,0.,0.));
#7791=DIRECTION('',(0.,0.,-1.));
#7792=DIRECTION('center_axis',(0.,0.,1.));
#7793=DIRECTION('ref_axis',(1.,0.,0.));
#7794=DIRECTION('center_axis',(0.809097497835397,0.587674432825267,5.7205382811039E-17));
#7795=DIRECTION('ref_axis',(1.84528382722603E-17,-1.22747433027317E-16,
1.));
#7796=DIRECTION('',(0.587674432825267,-0.809097497835397,0.));
#7797=DIRECTION('',(-0.470139546260214,0.647277998268318,0.6));
#7798=DIRECTION('',(0.,0.,1.));
#7799=DIRECTION('center_axis',(0.,0.,-1.));
#7800=DIRECTION('ref_axis',(-0.587674432825267,-0.809097497835397,0.));
#7801=DIRECTION('',(0.470139546260214,0.647277998268318,0.6));
#7802=DIRECTION('center_axis',(0.,0.,1.));
#7803=DIRECTION('ref_axis',(-0.587674432825267,-0.809097497835397,0.));
#7804=DIRECTION('center_axis',(0.,0.,1.));
#7805=DIRECTION('ref_axis',(-0.587674432825267,-0.809097497835397,0.));
#7806=DIRECTION('center_axis',(0.809097497835397,-0.587674432825267,5.7205382811039E-17));
#7807=DIRECTION('ref_axis',(-1.11022302462516E-16,-5.55111512312578E-17,
1.));
#7808=DIRECTION('',(0.587674432825267,0.809097497835397,0.));
#7809=DIRECTION('',(0.,0.,1.));
#7810=DIRECTION('center_axis',(0.8,-0.6,0.));
#7811=DIRECTION('ref_axis',(0.6,0.8,0.));
#7812=DIRECTION('',(0.,0.,-1.));
#7813=DIRECTION('',(0.6,0.8,0.));
#7814=DIRECTION('',(-0.6,-0.8,0.));
#7815=DIRECTION('center_axis',(0.6,0.8,0.));
#7816=DIRECTION('ref_axis',(-0.8,0.6,0.));
#7817=DIRECTION('',(0.8,-0.6,0.));
#7818=DIRECTION('',(0.,0.,1.));
#7819=DIRECTION('',(-0.8,0.6,0.));
#7820=DIRECTION('',(0.,0.,1.));
#7821=DIRECTION('center_axis',(0.,0.,1.));
#7822=DIRECTION('ref_axis',(4.44089209850063E-15,1.,0.));
#7823=DIRECTION('center_axis',(0.,0.,1.));
#7824=DIRECTION('ref_axis',(4.44089209850063E-15,1.,0.));
#7825=DIRECTION('center_axis',(0.,0.,1.));
#7826=DIRECTION('ref_axis',(4.44089209850063E-15,1.,0.));
#7827=DIRECTION('',(0.,0.,1.));
#7828=DIRECTION('center_axis',(0.,0.,1.));
#7829=DIRECTION('ref_axis',(-0.0832212223210449,0.996531097435194,0.));
#7830=DIRECTION('center_axis',(0.,0.,1.));
#7831=DIRECTION('ref_axis',(-0.0832212223210449,0.996531097435194,0.));
#7832=DIRECTION('center_axis',(0.,0.,1.));
#7833=DIRECTION('ref_axis',(-0.0832212223210449,0.996531097435194,0.));
#7834=DIRECTION('center_axis',(0.,0.,1.));
#7835=DIRECTION('ref_axis',(1.,0.,0.));
#7836=DIRECTION('',(0.,-1.,0.));
#7837=DIRECTION('',(-1.,0.,0.));
#7838=DIRECTION('center_axis',(0.,1.,0.));
#7839=DIRECTION('ref_axis',(-1.,0.,0.));
#7840=DIRECTION('',(0.,0.,1.));
#7841=DIRECTION('',(-1.,0.,0.));
#7842=DIRECTION('',(0.,0.,1.));
#7843=DIRECTION('',(1.,0.,0.));
#7844=DIRECTION('center_axis',(-1.,0.,0.));
#7845=DIRECTION('ref_axis',(0.,-1.,0.));
#7846=DIRECTION('',(0.,1.,0.));
#7847=DIRECTION('',(0.,0.,1.));
#7848=DIRECTION('',(0.,-1.,0.));
#7849=DIRECTION('center_axis',(0.,-1.,0.));
#7850=DIRECTION('ref_axis',(1.,0.,0.));
#7851=DIRECTION('',(0.,0.,-1.));
#7852=DIRECTION('',(1.,0.,0.));
#7853=DIRECTION('',(-1.,0.,0.));
#7854=DIRECTION('center_axis',(1.,0.,0.));
#7855=DIRECTION('ref_axis',(0.,1.,0.));
#7856=DIRECTION('',(0.,0.,1.));
#7857=DIRECTION('',(0.,-1.,0.));
#7858=DIRECTION('',(0.,1.,0.));
#7859=DIRECTION('center_axis',(0.,0.,1.));
#7860=DIRECTION('ref_axis',(1.,0.,0.));
#7861=DIRECTION('center_axis',(0.,0.,1.));
#7862=DIRECTION('ref_axis',(1.,0.,0.));
#7863=DIRECTION('',(0.,0.,1.));
#7864=DIRECTION('center_axis',(0.,0.,1.));
#7865=DIRECTION('ref_axis',(1.,0.,0.));
#7866=DIRECTION('center_axis',(0.,0.,1.));
#7867=DIRECTION('ref_axis',(1.,0.,0.));
#7868=DIRECTION('center_axis',(0.,0.,1.));
#7869=DIRECTION('ref_axis',(1.,0.,0.));
#7870=DIRECTION('',(0.,0.,-1.));
#7871=DIRECTION('center_axis',(0.,0.,1.));
#7872=DIRECTION('ref_axis',(1.,0.,0.));
#7873=DIRECTION('center_axis',(0.,0.,1.));
#7874=DIRECTION('ref_axis',(1.,0.,0.));
#7875=DIRECTION('',(0.865426285481126,-0.501036270541705,0.));
#7876=DIRECTION('center_axis',(0.,0.,1.));
#7877=DIRECTION('ref_axis',(1.,0.,0.));
#7878=DIRECTION('',(0.865426285481126,-0.501036270541705,0.));
#7879=DIRECTION('',(1.,0.,0.));
#7880=DIRECTION('',(0.,1.,0.));
#7881=DIRECTION('',(-1.,0.,0.));
#7882=DIRECTION('',(-0.707106781186548,0.707106781186548,0.));
#7883=DIRECTION('center_axis',(0.,0.,1.));
#7884=DIRECTION('ref_axis',(1.,0.,0.));
#7885=DIRECTION('',(-0.707106781186548,0.707106781186548,0.));
#7886=DIRECTION('',(-0.447213595499958,-0.894427190999916,0.));
#7887=DIRECTION('center_axis',(0.,0.,1.));
#7888=DIRECTION('ref_axis',(-1.,0.,0.));
#7889=DIRECTION('center_axis',(0.,0.,1.));
#7890=DIRECTION('ref_axis',(1.,0.,0.));
#7891=DIRECTION('center_axis',(0.,0.,-1.));
#7892=DIRECTION('ref_axis',(-1.,2.01858731750028E-16,0.));
#7893=DIRECTION('center_axis',(0.,-1.,0.));
#7894=DIRECTION('ref_axis',(-1.,0.,0.));
#7895=DIRECTION('center_axis',(0.,0.,1.));
#7896=DIRECTION('ref_axis',(-1.,2.01858731750028E-16,0.));
#7897=DIRECTION('center_axis',(0.,0.,-1.));
#7898=DIRECTION('ref_axis',(1.,0.,0.));
#7899=DIRECTION('center_axis',(0.,0.,-1.));
#7900=DIRECTION('ref_axis',(-1.,0.,0.));
#7901=DIRECTION('center_axis',(0.,0.,-1.));
#7902=DIRECTION('ref_axis',(-1.,0.,0.));
#7903=DIRECTION('',(0.,0.,-1.));
#7904=DIRECTION('center_axis',(0.,0.,1.));
#7905=DIRECTION('ref_axis',(1.,0.,0.));
#7906=DIRECTION('',(-0.447213595499958,-0.894427190999916,0.));
#7907=DIRECTION('',(-0.707106781186548,0.707106781186548,0.));
#7908=DIRECTION('center_axis',(0.,0.,1.));
#7909=DIRECTION('ref_axis',(1.,0.,0.));
#7910=DIRECTION('',(-0.707106781186548,0.707106781186548,0.));
#7911=DIRECTION('',(-1.,0.,0.));
#7912=DIRECTION('',(0.,1.,0.));
#7913=DIRECTION('',(1.,0.,0.));
#7914=DIRECTION('',(0.865426285481126,-0.501036270541705,0.));
#7915=DIRECTION('center_axis',(0.,0.,1.));
#7916=DIRECTION('ref_axis',(1.,0.,0.));
#7917=DIRECTION('',(0.865426285481126,-0.501036270541705,0.));
#7918=DIRECTION('center_axis',(0.,0.,-1.));
#7919=DIRECTION('ref_axis',(-1.,0.,0.));
#7920=DIRECTION('center_axis',(0.,-1.,0.));
#7921=DIRECTION('ref_axis',(1.,0.,0.));
#7922=DIRECTION('center_axis',(0.,0.,1.));
#7923=DIRECTION('ref_axis',(1.,0.,0.));
#7924=DIRECTION('',(0.,0.,-1.));
#7925=DIRECTION('',(0.,0.,1.));
#7926=DIRECTION('center_axis',(0.,0.,1.));
#7927=DIRECTION('ref_axis',(-0.501036270541705,-0.865426285481126,0.));
#7928=DIRECTION('',(0.,0.,1.));
#7929=DIRECTION('',(0.,0.,-1.));
#7930=DIRECTION('center_axis',(-0.501036270541705,-0.865426285481126,0.));
#7931=DIRECTION('ref_axis',(0.865426285481126,-0.501036270541705,0.));
#7932=DIRECTION('',(0.,0.,1.));
#7933=DIRECTION('center_axis',(0.707106781186548,0.707106781186548,0.));
#7934=DIRECTION('ref_axis',(-0.707106781186548,0.707106781186548,0.));
#7935=DIRECTION('',(0.,0.,1.));
#7936=DIRECTION('center_axis',(-0.501036270541705,-0.865426285481126,0.));
#7937=DIRECTION('ref_axis',(0.865426285481126,-0.501036270541705,0.));
#7938=DIRECTION('center_axis',(-0.894427190999916,0.447213595499958,0.));
#7939=DIRECTION('ref_axis',(-0.447213595499958,-0.894427190999916,0.));
#7940=DIRECTION('',(0.,0.,1.));
#7941=DIRECTION('center_axis',(0.707106781186548,0.707106781186548,0.));
#7942=DIRECTION('ref_axis',(-0.707106781186548,0.707106781186548,0.));
#7943=DIRECTION('center_axis',(0.,1.,0.));
#7944=DIRECTION('ref_axis',(-1.,0.,0.));
#7945=DIRECTION('',(0.,0.,1.));
#7946=DIRECTION('center_axis',(1.,0.,0.));
#7947=DIRECTION('ref_axis',(0.,1.,0.));
#7948=DIRECTION('',(0.,0.,1.));
#7949=DIRECTION('center_axis',(0.,-1.,0.));
#7950=DIRECTION('ref_axis',(1.,0.,0.));
#7951=DIRECTION('axis',(0.,0.,1.));
#7952=DIRECTION('refdir',(1.,0.,0.));
#7953=DIRECTION('center_axis',(0.,0.,-1.));
#7954=DIRECTION('ref_axis',(1.,0.,0.));
#7955=DIRECTION('center_axis',(0.,0.,-1.));
#7956=DIRECTION('ref_axis',(1.,0.,0.));
#7957=DIRECTION('',(0.,0.,-1.));
#7958=DIRECTION('center_axis',(0.,0.,1.));
#7959=DIRECTION('ref_axis',(1.,0.,0.));
#7960=DIRECTION('center_axis',(0.,0.,-1.));
#7961=DIRECTION('ref_axis',(1.,0.,0.));
#7962=DIRECTION('center_axis',(0.,0.,-1.));
#7963=DIRECTION('ref_axis',(1.,0.,0.));
#7964=DIRECTION('',(0.,0.,-1.));
#7965=DIRECTION('center_axis',(0.,0.,1.));
#7966=DIRECTION('ref_axis',(1.,0.,0.));
#7967=DIRECTION('center_axis',(0.,0.,-1.));
#7968=DIRECTION('ref_axis',(1.,0.,0.));
#7969=DIRECTION('center_axis',(0.,0.,-1.));
#7970=DIRECTION('ref_axis',(1.,0.,0.));
#7971=DIRECTION('',(0.,0.,-1.));
#7972=DIRECTION('center_axis',(0.,0.,1.));
#7973=DIRECTION('ref_axis',(1.,0.,0.));
#7974=DIRECTION('center_axis',(0.832050294337844,-0.554700196225229,0.));
#7975=DIRECTION('ref_axis',(0.554700196225229,0.832050294337844,0.));
#7976=DIRECTION('',(0.,0.,1.));
#7977=DIRECTION('',(0.554700196225229,0.832050294337844,0.));
#7978=DIRECTION('',(0.,0.,1.));
#7979=DIRECTION('',(-0.554700196225229,-0.832050294337844,0.));
#7980=DIRECTION('center_axis',(0.6,0.8,0.));
#7981=DIRECTION('ref_axis',(-0.8,0.6,0.));
#7982=DIRECTION('',(0.8,-0.6,0.));
#7983=DIRECTION('',(0.,0.,1.));
#7984=DIRECTION('',(-0.8,0.6,0.));
#7985=DIRECTION('',(0.,0.,1.));
#7986=DIRECTION('center_axis',(0.,0.,1.));
#7987=DIRECTION('ref_axis',(-0.667983855847227,-0.744175764404802,0.));
#7988=DIRECTION('center_axis',(0.,0.,1.));
#7989=DIRECTION('ref_axis',(-0.667983855847227,-0.744175764404802,0.));
#7990=DIRECTION('center_axis',(0.,0.,1.));
#7991=DIRECTION('ref_axis',(-0.667983855847227,-0.744175764404802,0.));
#7992=DIRECTION('',(0.,0.,1.));
#7993=DIRECTION('center_axis',(0.,0.,1.));
#7994=DIRECTION('ref_axis',(-2.96059473233375E-15,1.,0.));
#7995=DIRECTION('center_axis',(0.,0.,1.));
#7996=DIRECTION('ref_axis',(-2.96059473233375E-15,1.,0.));
#7997=DIRECTION('center_axis',(0.,0.,1.));
#7998=DIRECTION('ref_axis',(-2.96059473233375E-15,1.,0.));
#7999=DIRECTION('',(0.,0.,1.));
#8000=DIRECTION('center_axis',(0.,0.,1.));
#8001=DIRECTION('ref_axis',(-0.0846257248853095,0.99641280937553,0.));
#8002=DIRECTION('center_axis',(0.,0.,1.));
#8003=DIRECTION('ref_axis',(-0.0846257248853095,0.99641280937553,0.));
#8004=DIRECTION('center_axis',(0.,0.,1.));
#8005=DIRECTION('ref_axis',(-0.0846257248853095,0.99641280937553,0.));
#8006=DIRECTION('center_axis',(0.,0.,1.));
#8007=DIRECTION('ref_axis',(1.,0.,0.));
#8008=DIRECTION('',(-1.,0.,0.));
#8009=DIRECTION('',(0.,-1.,0.));
#8010=DIRECTION('center_axis',(0.,1.,0.));
#8011=DIRECTION('ref_axis',(-1.,0.,0.));
#8012=DIRECTION('',(0.,0.,1.));
#8013=DIRECTION('',(-1.,0.,0.));
#8014=DIRECTION('',(0.,0.,1.));
#8015=DIRECTION('',(1.,0.,0.));
#8016=DIRECTION('center_axis',(-1.,0.,0.));
#8017=DIRECTION('ref_axis',(0.,-1.,0.));
#8018=DIRECTION('',(0.,0.,1.));
#8019=DIRECTION('',(0.,-1.,0.));
#8020=DIRECTION('center_axis',(0.,-1.,0.));
#8021=DIRECTION('ref_axis',(1.,0.,0.));
#8022=DIRECTION('',(0.,0.,-1.));
#8023=DIRECTION('',(1.,0.,0.));
#8024=DIRECTION('',(-1.,0.,0.));
#8025=DIRECTION('center_axis',(1.,0.,0.));
#8026=DIRECTION('ref_axis',(0.,1.,0.));
#8027=DIRECTION('',(0.,0.,1.));
#8028=DIRECTION('',(0.,-1.,0.));
#8029=DIRECTION('',(0.,1.,0.));
#8030=DIRECTION('center_axis',(0.,0.,1.));
#8031=DIRECTION('ref_axis',(1.,0.,0.));
#8032=DIRECTION('center_axis',(0.,0.,1.));
#8033=DIRECTION('ref_axis',(1.,0.,0.));
#8034=DIRECTION('',(0.,0.,1.));
#8035=DIRECTION('center_axis',(0.,0.,1.));
#8036=DIRECTION('ref_axis',(1.,0.,0.));
#8037=DIRECTION('center_axis',(0.,0.,1.));
#8038=DIRECTION('ref_axis',(1.,0.,0.));
#8039=DIRECTION('center_axis',(0.,0.,1.));
#8040=DIRECTION('ref_axis',(1.,0.,0.));
#8041=DIRECTION('',(0.,0.,-1.));
#8042=DIRECTION('center_axis',(0.,0.,1.));
#8043=DIRECTION('ref_axis',(1.,0.,0.));
#8044=DIRECTION('center_axis',(0.,0.,1.));
#8045=DIRECTION('ref_axis',(1.,0.,0.));
#8046=DIRECTION('',(0.865426285481126,-0.501036270541705,0.));
#8047=DIRECTION('center_axis',(0.,0.,1.));
#8048=DIRECTION('ref_axis',(1.,0.,0.));
#8049=DIRECTION('',(0.865426285481126,-0.501036270541705,0.));
#8050=DIRECTION('',(1.,0.,0.));
#8051=DIRECTION('',(0.,1.,0.));
#8052=DIRECTION('',(-1.,0.,0.));
#8053=DIRECTION('',(-0.707106781186548,0.707106781186548,0.));
#8054=DIRECTION('center_axis',(0.,0.,1.));
#8055=DIRECTION('ref_axis',(1.,0.,0.));
#8056=DIRECTION('',(-0.707106781186548,0.707106781186548,0.));
#8057=DIRECTION('',(-0.447213595499958,-0.894427190999916,0.));
#8058=DIRECTION('center_axis',(0.,0.,1.));
#8059=DIRECTION('ref_axis',(-1.,0.,0.));
#8060=DIRECTION('center_axis',(0.,0.,1.));
#8061=DIRECTION('ref_axis',(1.,0.,0.));
#8062=DIRECTION('center_axis',(0.,0.,-1.));
#8063=DIRECTION('ref_axis',(-1.,2.01858731750028E-16,0.));
#8064=DIRECTION('center_axis',(0.,-1.,0.));
#8065=DIRECTION('ref_axis',(-1.,0.,0.));
#8066=DIRECTION('center_axis',(0.,0.,1.));
#8067=DIRECTION('ref_axis',(-1.,2.01858731750028E-16,0.));
#8068=DIRECTION('center_axis',(0.,0.,-1.));
#8069=DIRECTION('ref_axis',(1.,0.,0.));
#8070=DIRECTION('center_axis',(0.,0.,-1.));
#8071=DIRECTION('ref_axis',(-1.,0.,0.));
#8072=DIRECTION('center_axis',(0.,0.,-1.));
#8073=DIRECTION('ref_axis',(-1.,0.,0.));
#8074=DIRECTION('',(0.,0.,-1.));
#8075=DIRECTION('center_axis',(0.,0.,1.));
#8076=DIRECTION('ref_axis',(1.,0.,0.));
#8077=DIRECTION('',(-0.447213595499958,-0.894427190999916,0.));
#8078=DIRECTION('',(-0.707106781186548,0.707106781186548,0.));
#8079=DIRECTION('center_axis',(0.,0.,1.));
#8080=DIRECTION('ref_axis',(1.,0.,0.));
#8081=DIRECTION('',(-0.707106781186548,0.707106781186548,0.));
#8082=DIRECTION('',(-1.,0.,0.));
#8083=DIRECTION('',(0.,1.,0.));
#8084=DIRECTION('',(1.,0.,0.));
#8085=DIRECTION('',(0.865426285481126,-0.501036270541705,0.));
#8086=DIRECTION('center_axis',(0.,0.,1.));
#8087=DIRECTION('ref_axis',(1.,0.,0.));
#8088=DIRECTION('',(0.865426285481126,-0.501036270541705,0.));
#8089=DIRECTION('center_axis',(0.,0.,-1.));
#8090=DIRECTION('ref_axis',(-1.,0.,0.));
#8091=DIRECTION('center_axis',(0.,-1.,0.));
#8092=DIRECTION('ref_axis',(1.,0.,0.));
#8093=DIRECTION('center_axis',(0.,0.,1.));
#8094=DIRECTION('ref_axis',(1.,0.,0.));
#8095=DIRECTION('',(0.,0.,-1.));
#8096=DIRECTION('',(0.,0.,1.));
#8097=DIRECTION('center_axis',(0.,0.,1.));
#8098=DIRECTION('ref_axis',(-0.501036270541705,-0.865426285481126,0.));
#8099=DIRECTION('',(0.,0.,1.));
#8100=DIRECTION('',(0.,0.,-1.));
#8101=DIRECTION('center_axis',(-0.501036270541705,-0.865426285481126,0.));
#8102=DIRECTION('ref_axis',(0.865426285481126,-0.501036270541705,0.));
#8103=DIRECTION('',(0.,0.,1.));
#8104=DIRECTION('center_axis',(0.707106781186548,0.707106781186548,0.));
#8105=DIRECTION('ref_axis',(-0.707106781186548,0.707106781186548,0.));
#8106=DIRECTION('',(0.,0.,1.));
#8107=DIRECTION('center_axis',(-0.501036270541705,-0.865426285481126,0.));
#8108=DIRECTION('ref_axis',(0.865426285481126,-0.501036270541705,0.));
#8109=DIRECTION('center_axis',(-0.894427190999916,0.447213595499958,0.));
#8110=DIRECTION('ref_axis',(-0.447213595499958,-0.894427190999916,0.));
#8111=DIRECTION('',(0.,0.,1.));
#8112=DIRECTION('center_axis',(0.707106781186548,0.707106781186548,0.));
#8113=DIRECTION('ref_axis',(-0.707106781186548,0.707106781186548,0.));
#8114=DIRECTION('center_axis',(0.,1.,0.));
#8115=DIRECTION('ref_axis',(-1.,0.,0.));
#8116=DIRECTION('',(0.,0.,1.));
#8117=DIRECTION('center_axis',(1.,0.,0.));
#8118=DIRECTION('ref_axis',(0.,1.,0.));
#8119=DIRECTION('',(0.,0.,1.));
#8120=DIRECTION('center_axis',(0.,-1.,0.));
#8121=DIRECTION('ref_axis',(1.,0.,0.));
#8122=DIRECTION('axis',(0.,0.,1.));
#8123=DIRECTION('refdir',(1.,0.,0.));
#8124=DIRECTION('center_axis',(0.,0.,1.));
#8125=DIRECTION('ref_axis',(1.,0.,0.));
#8126=DIRECTION('center_axis',(0.,0.,1.));
#8127=DIRECTION('ref_axis',(1.,0.,0.));
#8128=DIRECTION('',(0.,0.,1.));
#8129=DIRECTION('center_axis',(0.,0.,1.));
#8130=DIRECTION('ref_axis',(1.,0.,0.));
#8131=DIRECTION('center_axis',(0.,0.,-1.));
#8132=DIRECTION('ref_axis',(-1.,0.,0.));
#8133=DIRECTION('center_axis',(0.,0.,-1.));
#8134=DIRECTION('ref_axis',(1.,0.,0.));
#8135=DIRECTION('center_axis',(0.,0.,1.));
#8136=DIRECTION('ref_axis',(1.,0.,0.));
#8137=DIRECTION('center_axis',(0.,0.,1.));
#8138=DIRECTION('ref_axis',(1.,0.,0.));
#8139=DIRECTION('center_axis',(0.,0.,1.));
#8140=DIRECTION('ref_axis',(1.,0.,0.));
#8141=DIRECTION('center_axis',(0.,0.,1.));
#8142=DIRECTION('ref_axis',(1.,0.,0.));
#8143=DIRECTION('',(0.,0.,-1.));
#8144=DIRECTION('center_axis',(0.,0.,1.));
#8145=DIRECTION('ref_axis',(1.,0.,0.));
#8146=DIRECTION('center_axis',(0.,0.,1.));
#8147=DIRECTION('ref_axis',(1.,0.,0.));
#8148=DIRECTION('center_axis',(0.,0.,1.));
#8149=DIRECTION('ref_axis',(1.,0.,0.));
#8150=DIRECTION('center_axis',(0.,0.,1.));
#8151=DIRECTION('ref_axis',(1.,0.,0.));
#8152=DIRECTION('',(0.,0.,-1.));
#8153=DIRECTION('center_axis',(0.,0.,1.));
#8154=DIRECTION('ref_axis',(1.,0.,0.));
#8155=DIRECTION('center_axis',(0.,0.,1.));
#8156=DIRECTION('ref_axis',(1.,0.,0.));
#8157=DIRECTION('center_axis',(0.,0.,1.));
#8158=DIRECTION('ref_axis',(1.,0.,0.));
#8159=DIRECTION('',(0.,0.,-1.));
#8160=DIRECTION('center_axis',(0.,0.,1.));
#8161=DIRECTION('ref_axis',(1.,0.,0.));
#8162=DIRECTION('axis',(0.,0.,1.));
#8163=DIRECTION('refdir',(1.,0.,0.));
#8164=DIRECTION('center_axis',(-1.,0.,0.));
#8165=DIRECTION('ref_axis',(0.,1.,0.));
#8166=DIRECTION('',(0.,0.,1.));
#8167=DIRECTION('',(0.,-1.,0.));
#8168=DIRECTION('',(0.,0.,-1.));
#8169=DIRECTION('',(0.,1.,0.));
#8170=DIRECTION('center_axis',(1.,0.,0.));
#8171=DIRECTION('ref_axis',(0.,-1.,0.));
#8172=DIRECTION('',(0.,0.,-1.));
#8173=DIRECTION('',(0.,-1.,0.));
#8174=DIRECTION('',(0.,0.,1.));
#8175=DIRECTION('',(0.,1.,0.));
#8176=DIRECTION('center_axis',(0.,0.,1.));
#8177=DIRECTION('ref_axis',(1.,0.,0.));
#8178=DIRECTION('center_axis',(0.,0.,1.));
#8179=DIRECTION('ref_axis',(1.,0.,0.));
#8180=DIRECTION('center_axis',(0.,0.,-1.));
#8181=DIRECTION('ref_axis',(1.,0.,0.));
#8182=DIRECTION('center_axis',(0.,0.,1.));
#8183=DIRECTION('ref_axis',(6.12323399573677E-17,-1.,0.));
#8184=DIRECTION('center_axis',(0.,0.,-1.));
#8185=DIRECTION('ref_axis',(1.,0.,0.));
#8186=DIRECTION('center_axis',(0.,0.,1.));
#8187=DIRECTION('ref_axis',(6.12323399573677E-17,-1.,0.));
#8188=DIRECTION('center_axis',(0.,0.,1.));
#8189=DIRECTION('ref_axis',(1.,0.,0.));
#8190=DIRECTION('center_axis',(0.,0.,1.));
#8191=DIRECTION('ref_axis',(1.,0.,0.));
#8192=DIRECTION('axis',(0.,0.,1.));
#8193=DIRECTION('refdir',(1.,0.,0.));
#8194=DIRECTION('axis',(0.,0.,1.));
#8195=DIRECTION('refdir',(1.,0.,0.));
#8196=DIRECTION('center_axis',(-9.61618982193066E-33,1.03600583455278E-18,
1.));
#8197=DIRECTION('ref_axis',(1.,0.,9.61618982193066E-33));
#8198=DIRECTION('',(0.,-1.,1.03600583455278E-18));
#8199=DIRECTION('',(0.,1.,-1.03600583455278E-18));
#8200=DIRECTION('center_axis',(-9.61618982193066E-33,1.03600583455278E-18,
1.));
#8201=DIRECTION('ref_axis',(1.,0.,0.));
#8202=DIRECTION('center_axis',(-9.61618982193066E-33,1.03600583455278E-18,
1.));
#8203=DIRECTION('ref_axis',(1.,0.,0.));
#8204=DIRECTION('center_axis',(-9.61618982193066E-33,1.03600583455278E-18,
1.));
#8205=DIRECTION('ref_axis',(1.,0.,0.));
#8206=DIRECTION('center_axis',(0.,0.,-1.));
#8207=DIRECTION('ref_axis',(1.,0.,0.));
#8208=DIRECTION('center_axis',(9.61618982193066E-33,-1.03600583455278E-18,
-1.));
#8209=DIRECTION('ref_axis',(1.,0.,0.));
#8210=DIRECTION('',(0.,0.,-1.));
#8211=DIRECTION('center_axis',(-9.61618982193066E-33,1.03600583455278E-18,
1.));
#8212=DIRECTION('ref_axis',(1.,0.,0.));
#8213=DIRECTION('center_axis',(0.,0.,-1.));
#8214=DIRECTION('ref_axis',(1.,0.,0.));
#8215=DIRECTION('center_axis',(9.61618982193066E-33,-1.03600583455278E-18,
-1.));
#8216=DIRECTION('ref_axis',(1.,0.,0.));
#8217=DIRECTION('',(0.,0.,-1.));
#8218=DIRECTION('center_axis',(0.,0.,-1.));
#8219=DIRECTION('ref_axis',(1.,0.,0.));
#8220=DIRECTION('center_axis',(9.61618982193066E-33,-1.03600583455278E-18,
-1.));
#8221=DIRECTION('ref_axis',(1.,0.,0.));
#8222=DIRECTION('',(0.,0.,-1.));
#8223=DIRECTION('center_axis',(0.,0.,-1.));
#8224=DIRECTION('ref_axis',(1.,0.,0.));
#8225=DIRECTION('center_axis',(9.61618982193066E-33,-1.03600583455278E-18,
-1.));
#8226=DIRECTION('ref_axis',(1.,0.,0.));
#8227=DIRECTION('',(0.,0.,-1.));
#8228=DIRECTION('center_axis',(-9.61618982193066E-33,1.03600583455278E-18,
1.));
#8229=DIRECTION('ref_axis',(1.,0.,0.));
#8230=DIRECTION('center_axis',(0.,0.,-1.));
#8231=DIRECTION('ref_axis',(1.,0.,0.));
#8232=DIRECTION('center_axis',(9.61618982193066E-33,-1.03600583455278E-18,
-1.));
#8233=DIRECTION('ref_axis',(1.,0.,0.));
#8234=DIRECTION('',(0.,0.,-1.));
#8235=DIRECTION('center_axis',(0.,0.,-1.));
#8236=DIRECTION('ref_axis',(1.,0.,0.));
#8237=DIRECTION('center_axis',(0.,0.,-1.));
#8238=DIRECTION('ref_axis',(1.,0.,0.));
#8239=DIRECTION('center_axis',(0.,0.,1.));
#8240=DIRECTION('ref_axis',(1.,0.,0.));
#8241=DIRECTION('center_axis',(0.,0.,-1.));
#8242=DIRECTION('ref_axis',(1.,0.,0.));
#8243=DIRECTION('center_axis',(9.61618982193066E-33,-1.03600583455278E-18,
-1.));
#8244=DIRECTION('ref_axis',(1.,0.,0.));
#8245=DIRECTION('',(0.,0.,-1.));
#8246=DIRECTION('center_axis',(0.,0.,-1.));
#8247=DIRECTION('ref_axis',(1.,0.,0.));
#8248=DIRECTION('center_axis',(0.,0.,-1.));
#8249=DIRECTION('ref_axis',(1.,0.,0.));
#8250=DIRECTION('center_axis',(0.,0.,1.));
#8251=DIRECTION('ref_axis',(1.,0.,0.));
#8252=DIRECTION('center_axis',(0.,0.,-1.));
#8253=DIRECTION('ref_axis',(1.,0.,0.));
#8254=DIRECTION('',(0.,0.,-1.));
#8255=DIRECTION('center_axis',(0.,0.,1.));
#8256=DIRECTION('ref_axis',(1.,0.,0.));
#8257=DIRECTION('center_axis',(0.,0.,-1.));
#8258=DIRECTION('ref_axis',(1.,0.,0.));
#8259=DIRECTION('',(0.,0.,-1.));
#8260=DIRECTION('center_axis',(0.,0.,1.));
#8261=DIRECTION('ref_axis',(1.,0.,0.));
#8262=DIRECTION('center_axis',(0.,-1.,0.));
#8263=DIRECTION('ref_axis',(-1.,0.,0.));
#8264=DIRECTION('',(0.0523359562429438,0.,0.998629534754574));
#8265=DIRECTION('',(1.,0.,0.));
#8266=DIRECTION('',(-0.0523359562429438,0.,-0.998629534754574));
#8267=DIRECTION('',(1.,0.,0.));
#8268=DIRECTION('center_axis',(0.,-1.,0.));
#8269=DIRECTION('ref_axis',(-1.,0.,0.));
#8270=DIRECTION('',(0.,0.,-1.));
#8271=DIRECTION('',(1.,0.,0.));
#8272=DIRECTION('',(0.,0.,1.));
#8273=DIRECTION('',(1.,0.,0.));
#8274=DIRECTION('center_axis',(0.,-1.,0.));
#8275=DIRECTION('ref_axis',(-1.,0.,0.));
#8276=DIRECTION('',(0.,0.,-1.));
#8277=DIRECTION('',(1.,0.,0.));
#8278=DIRECTION('',(0.,0.,1.));
#8279=DIRECTION('',(1.,0.,0.));
#8280=DIRECTION('center_axis',(0.,-1.,0.));
#8281=DIRECTION('ref_axis',(-1.,0.,0.));
#8282=DIRECTION('',(0.,0.,-1.));
#8283=DIRECTION('',(1.,0.,0.));
#8284=DIRECTION('',(0.,0.,1.));
#8285=DIRECTION('',(1.,0.,0.));
#8286=DIRECTION('center_axis',(0.,1.,0.));
#8287=DIRECTION('ref_axis',(1.,0.,0.));
#8288=DIRECTION('',(-0.0523359562429438,0.,-0.998629534754574));
#8289=DIRECTION('',(-1.,0.,0.));
#8290=DIRECTION('',(0.0523359562429438,0.,0.998629534754574));
#8291=DIRECTION('',(-1.,0.,0.));
#8292=DIRECTION('center_axis',(0.,1.,0.));
#8293=DIRECTION('ref_axis',(1.,0.,0.));
#8294=DIRECTION('',(0.,0.,1.));
#8295=DIRECTION('',(-1.,0.,0.));
#8296=DIRECTION('',(0.,0.,-1.));
#8297=DIRECTION('',(-1.,0.,0.));
#8298=DIRECTION('center_axis',(0.,1.,0.));
#8299=DIRECTION('ref_axis',(1.,0.,0.));
#8300=DIRECTION('',(0.,0.,1.));
#8301=DIRECTION('',(-1.,0.,0.));
#8302=DIRECTION('',(0.,0.,-1.));
#8303=DIRECTION('',(-1.,0.,0.));
#8304=DIRECTION('center_axis',(0.,0.,1.));
#8305=DIRECTION('ref_axis',(1.,0.,0.));
#8306=DIRECTION('center_axis',(0.,0.,1.));
#8307=DIRECTION('ref_axis',(1.,0.,0.));
#8308=DIRECTION('center_axis',(0.,0.,1.));
#8309=DIRECTION('ref_axis',(1.,0.,0.));
#8310=DIRECTION('center_axis',(0.,0.,1.));
#8311=DIRECTION('ref_axis',(1.,0.,0.));
#8312=DIRECTION('center_axis',(0.,0.,1.));
#8313=DIRECTION('ref_axis',(1.,0.,0.));
#8314=DIRECTION('',(0.,1.,0.));
#8315=DIRECTION('',(0.,-1.,0.));
#8316=DIRECTION('center_axis',(0.,0.,1.));
#8317=DIRECTION('ref_axis',(1.,0.,0.));
#8318=DIRECTION('',(0.,-1.,0.));
#8319=DIRECTION('',(0.,1.,0.));
#8320=DIRECTION('center_axis',(0.,0.,1.));
#8321=DIRECTION('ref_axis',(1.,0.,0.));
#8322=DIRECTION('',(0.,-1.,0.));
#8323=DIRECTION('',(0.,1.,0.));
#8324=DIRECTION('center_axis',(0.,0.,1.));
#8325=DIRECTION('ref_axis',(1.,0.,0.));
#8326=DIRECTION('',(0.,-1.,0.));
#8327=DIRECTION('',(-1.,0.,0.));
#8328=DIRECTION('',(0.,1.,0.));
#8329=DIRECTION('center_axis',(0.,1.,0.));
#8330=DIRECTION('ref_axis',(1.,0.,0.));
#8331=DIRECTION('',(0.,0.,1.));
#8332=DIRECTION('',(-1.,0.,0.));
#8333=DIRECTION('',(0.,0.,-1.));
#8334=DIRECTION('center_axis',(-1.,0.,0.));
#8335=DIRECTION('ref_axis',(0.,-1.,0.));
#8336=DIRECTION('',(0.,-1.,0.));
#8337=DIRECTION('',(0.,-1.,1.03600583455278E-18));
#8338=DIRECTION('center_axis',(1.,0.,0.));
#8339=DIRECTION('ref_axis',(0.,1.,0.));
#8340=DIRECTION('',(0.,1.,0.));
#8341=DIRECTION('',(0.,1.,-1.03600583455278E-18));
#8342=DIRECTION('',(0.,1.,0.));
#8343=DIRECTION('center_axis',(1.,0.,0.));
#8344=DIRECTION('ref_axis',(0.,1.,0.));
#8345=DIRECTION('',(0.,1.,0.));
#8346=DIRECTION('',(0.,1.,-1.03600583455278E-18));
#8347=DIRECTION('',(0.,1.,0.));
#8348=DIRECTION('center_axis',(1.,0.,0.));
#8349=DIRECTION('ref_axis',(0.,1.,0.));
#8350=DIRECTION('',(0.,1.,0.));
#8351=DIRECTION('',(0.,1.,0.));
#8352=DIRECTION('center_axis',(0.998629534754574,0.,-0.0523359562429438));
#8353=DIRECTION('ref_axis',(-0.0523359562429438,0.,-0.998629534754574));
#8354=DIRECTION('',(0.,-1.,0.));
#8355=DIRECTION('',(5.42947651131849E-20,-1.,1.03600583455278E-18));
#8356=DIRECTION('',(0.,-1.,0.));
#8357=DIRECTION('center_axis',(0.,0.,1.));
#8358=DIRECTION('ref_axis',(1.,0.,0.));
#8359=DIRECTION('',(0.,-1.,0.));
#8360=DIRECTION('',(0.,-1.,0.));
#8361=DIRECTION('',(0.,-1.,0.));
#8362=DIRECTION('',(0.,1.,0.));
#8363=DIRECTION('',(0.,-1.,0.));
#8364=DIRECTION('',(0.,1.,0.));
#8365=DIRECTION('',(0.,-1.,0.));
#8366=DIRECTION('',(0.,-1.,0.));
#8367=DIRECTION('',(0.,-1.,0.));
#8368=DIRECTION('',(0.,1.,0.));
#8369=DIRECTION('',(0.,1.,0.));
#8370=DIRECTION('center_axis',(0.,0.,1.));
#8371=DIRECTION('ref_axis',(1.,0.,0.));
#8372=DIRECTION('center_axis',(-9.61618982193066E-33,1.03600583455278E-18,
1.));
#8373=DIRECTION('ref_axis',(1.,0.,0.));
#8374=DIRECTION('',(0.,0.,-1.));
#8375=DIRECTION('center_axis',(0.,0.,1.));
#8376=DIRECTION('ref_axis',(1.,0.,0.));
#8377=DIRECTION('',(0.,0.,-1.));
#8378=DIRECTION('center_axis',(1.,0.,0.));
#8379=DIRECTION('ref_axis',(0.,1.,0.));
#8380=DIRECTION('',(0.,1.,-1.03600583455278E-18));
#8381=DIRECTION('center_axis',(0.994044372876412,-0.108976074221552,-1.1933167131821E-14));
#8382=DIRECTION('ref_axis',(-0.108857570442347,-0.992963419871597,0.0466226999892957));
#8383=DIRECTION('center_axis',(-9.61618982193066E-33,1.03600583455278E-18,
1.));
#8384=DIRECTION('ref_axis',(1.,0.,9.61618982193066E-33));
#8385=DIRECTION('center_axis',(-9.61618982193066E-33,1.03600583455278E-18,
1.));
#8386=DIRECTION('ref_axis',(1.,0.,9.61618982193066E-33));
#8387=DIRECTION('',(-5.42947651131849E-20,-1.,1.03600583455278E-18));
#8388=DIRECTION('center_axis',(-1.,0.,0.));
#8389=DIRECTION('ref_axis',(0.,-1.,0.));
#8390=DIRECTION('',(0.,-1.,1.03600583455278E-18));
#8391=DIRECTION('center_axis',(-9.61618982193066E-33,1.03600583455278E-18,
1.));
#8392=DIRECTION('ref_axis',(1.,0.,9.61618982193066E-33));
#8393=DIRECTION('center_axis',(-1.,0.,0.));
#8394=DIRECTION('ref_axis',(0.,-1.,0.));
#8395=DIRECTION('center_axis',(-1.,0.,0.));
#8396=DIRECTION('ref_axis',(0.,-1.,0.));
#8397=DIRECTION('',(0.,-1.,1.03600583455278E-18));
#8398=DIRECTION('center_axis',(-0.999738255753194,0.0228783737088345,0.));
#8399=DIRECTION('ref_axis',(0.,0.,1.));
#8400=DIRECTION('center_axis',(-9.61618982193066E-33,1.03600583455278E-18,
1.));
#8401=DIRECTION('ref_axis',(1.,0.,9.61618982193066E-33));
#8402=DIRECTION('',(-5.42947651131849E-20,1.,-1.03600583455278E-18));
#8403=DIRECTION('center_axis',(-0.999738255790058,-0.0228783720979604,1.69987959829136E-9));
#8404=DIRECTION('ref_axis',(-0.022845652001536,0.998308458201847,0.0534630570326489));
#8405=DIRECTION('center_axis',(-0.375013085256251,-0.833398400631247,0.405970801550885));
#8406=DIRECTION('ref_axis',(-0.565498005067694,0.552672693214782,0.612180447612612));
#8407=DIRECTION('center_axis',(-7.78474640228738E-11,1.,0.));
#8408=DIRECTION('ref_axis',(0.,0.,1.));
#8409=DIRECTION('center_axis',(0.0522645732252412,-0.0522112666801462,0.997267465636596));
#8410=DIRECTION('ref_axis',(-0.998629534754574,0.,0.0523359562429445));
#8411=DIRECTION('center_axis',(0.361627795167438,-0.818371417997736,0.44664701943113));
#8412=DIRECTION('ref_axis',(0.514966362801186,0.574689674697898,0.636035708886648));
#8413=DIRECTION('center_axis',(0.994044372876412,0.108976074221546,-5.96658356591051E-15));
#8414=DIRECTION('ref_axis',(5.9211894646675E-15,7.40148683083438E-16,1.));
#8415=DIRECTION('center_axis',(-0.052263633556273,-0.0525535553916586,0.997249535684621));
#8416=DIRECTION('ref_axis',(-0.108857570442347,0.992963419871597,0.0466226999892949));
#8417=DIRECTION('center_axis',(0.,1.,0.));
#8418=DIRECTION('ref_axis',(0.998629534754574,0.,0.0523359562429438));
#8419=DIRECTION('center_axis',(0.375013085403515,-0.833398400816333,-0.405970801034895));
#8420=DIRECTION('ref_axis',(-0.565498005700927,-0.552672692935682,0.612180447279637));
#8421=DIRECTION('center_axis',(0.0522645732252408,0.0522112666801459,0.997267465636596));
#8422=DIRECTION('ref_axis',(-0.0228456520015352,-0.998308458201847,0.0534630570326489));
#8423=DIRECTION('center_axis',(-4.07418268117644E-12,-1.,-7.77400366303027E-11));
#8424=DIRECTION('ref_axis',(-0.998629534754574,0.,0.0523359562429438));
#8425=DIRECTION('center_axis',(-5.42947651131849E-20,1.,-1.03600583455278E-18));
#8426=DIRECTION('ref_axis',(-0.688354575693754,0.,0.725374371012288));
#8427=DIRECTION('center_axis',(-0.361627795167436,-0.818371417997736,-0.446647019431131));
#8428=DIRECTION('ref_axis',(0.514966362801185,-0.574689674697896,0.636035708886651));
#8429=DIRECTION('center_axis',(-0.0522636335562752,0.0525535553916633,0.99724953568462));
#8430=DIRECTION('ref_axis',(0.998629534754574,0.,0.0523359562429442));
#8431=DIRECTION('center_axis',(0.,-1.,0.));
#8432=DIRECTION('ref_axis',(0.,0.,1.));
#8433=DIRECTION('center_axis',(-5.42947651131849E-20,-1.,1.03600583455278E-18));
#8434=DIRECTION('ref_axis',(0.688354575693754,0.,0.725374371012288));
#8435=DIRECTION('',(5.42947651131849E-20,1.,-1.03600583455278E-18));
#8436=DIRECTION('center_axis',(-0.998629534754574,0.,-0.0523359562429438));
#8437=DIRECTION('ref_axis',(-0.0523359562429438,0.,0.998629534754574));
#8438=DIRECTION('center_axis',(-0.375013085256251,-0.833398400631247,0.405970801550885));
#8439=DIRECTION('ref_axis',(-0.565498005067695,0.552672693214781,0.612180447612612));
#8440=DIRECTION('center_axis',(-7.78474640228738E-11,1.,0.));
#8441=DIRECTION('ref_axis',(0.,0.,1.));
#8442=DIRECTION('center_axis',(-0.999738255790058,-0.0228783720979604,1.69987959829136E-9));
#8443=DIRECTION('ref_axis',(-0.022845652001536,0.998308458201847,0.0534630570326489));
#8444=DIRECTION('center_axis',(0.0522645732252412,-0.0522112666801462,0.997267465636596));
#8445=DIRECTION('ref_axis',(-0.998629534754574,0.,0.0523359562429445));
#8446=DIRECTION('center_axis',(0.361627795167442,-0.818371417997735,0.446647019431129));
#8447=DIRECTION('ref_axis',(0.514966362801186,0.574689674697898,0.636035708886649));
#8448=DIRECTION('center_axis',(0.994044372876412,0.108976074221546,-5.96658356591051E-15));
#8449=DIRECTION('ref_axis',(5.9211894646675E-15,7.40148683083438E-16,1.));
#8450=DIRECTION('center_axis',(0.,1.,0.));
#8451=DIRECTION('ref_axis',(0.998629534754574,0.,0.0523359562429438));
#8452=DIRECTION('center_axis',(-0.052263633556273,-0.0525535553916586,0.997249535684621));
#8453=DIRECTION('ref_axis',(-0.108857570442347,0.992963419871597,0.0466226999892949));
#8454=DIRECTION('center_axis',(0.375013085403515,-0.833398400816333,-0.405970801034895));
#8455=DIRECTION('ref_axis',(-0.565498005700926,-0.552672692935682,0.612180447279637));
#8456=DIRECTION('center_axis',(-0.999738255753194,0.0228783737088345,0.));
#8457=DIRECTION('ref_axis',(0.,0.,1.));
#8458=DIRECTION('center_axis',(-4.07418268117644E-12,-1.,-7.77400366303027E-11));
#8459=DIRECTION('ref_axis',(-0.998629534754574,0.,0.0523359562429438));
#8460=DIRECTION('center_axis',(0.0522645732252408,0.0522112666801459,0.997267465636596));
#8461=DIRECTION('ref_axis',(-0.0228456520015352,-0.998308458201847,0.0534630570326489));
#8462=DIRECTION('center_axis',(-5.42947651131849E-20,1.,-1.03600583455278E-18));
#8463=DIRECTION('ref_axis',(-0.688354575693754,0.,0.725374371012288));
#8464=DIRECTION('',(5.42947651131849E-20,-1.,1.03600583455278E-18));
#8465=DIRECTION('',(-5.42947651131849E-20,1.,-1.03600583455278E-18));
#8466=DIRECTION('center_axis',(-0.361627795167436,-0.818371417997736,-0.446647019431131));
#8467=DIRECTION('ref_axis',(0.51496636280118,-0.574689674697898,0.636035708886653));
#8468=DIRECTION('center_axis',(-0.0522636335562752,0.0525535553916633,0.99724953568462));
#8469=DIRECTION('ref_axis',(0.998629534754574,0.,0.0523359562429441));
#8470=DIRECTION('center_axis',(0.,-1.,0.));
#8471=DIRECTION('ref_axis',(0.,0.,1.));
#8472=DIRECTION('center_axis',(0.994044372876412,-0.108976074221552,-1.1933167131821E-14));
#8473=DIRECTION('ref_axis',(-0.108857570442347,-0.992963419871597,0.0466226999892957));
#8474=DIRECTION('center_axis',(-5.42947651131849E-20,-1.,1.03600583455278E-18));
#8475=DIRECTION('ref_axis',(0.688354575693754,0.,0.725374371012288));
#8476=DIRECTION('',(5.42947651131849E-20,1.,-1.03600583455278E-18));
#8477=DIRECTION('',(-5.42947651131849E-20,-1.,1.03600583455278E-18));
#8478=DIRECTION('center_axis',(0.998629534754574,0.,-0.0523359562429438));
#8479=DIRECTION('ref_axis',(-0.0523359562429438,0.,-0.998629534754574));
#8480=DIRECTION('center_axis',(-9.61618982193066E-33,1.03600583455278E-18,
1.));
#8481=DIRECTION('ref_axis',(1.,0.,9.61618982193066E-33));
#8482=DIRECTION('center_axis',(-0.998629534754574,0.,-0.0523359562429438));
#8483=DIRECTION('ref_axis',(-0.0523359562429438,0.,0.998629534754574));
#8484=DIRECTION('axis',(0.,0.,1.));
#8485=DIRECTION('refdir',(1.,0.,0.));
#8486=DIRECTION('center_axis',(-9.61618982193066E-33,1.03600583455278E-18,
1.));
#8487=DIRECTION('ref_axis',(1.,0.,9.61618982193066E-33));
#8488=DIRECTION('',(0.,-1.,1.03600583455278E-18));
#8489=DIRECTION('',(0.,1.,-1.03600583455278E-18));
#8490=DIRECTION('center_axis',(-9.61618982193066E-33,1.03600583455278E-18,
1.));
#8491=DIRECTION('ref_axis',(1.,0.,0.));
#8492=DIRECTION('center_axis',(-9.61618982193066E-33,1.03600583455278E-18,
1.));
#8493=DIRECTION('ref_axis',(1.,0.,0.));
#8494=DIRECTION('center_axis',(-9.61618982193066E-33,1.03600583455278E-18,
1.));
#8495=DIRECTION('ref_axis',(1.,0.,0.));
#8496=DIRECTION('center_axis',(0.,0.,-1.));
#8497=DIRECTION('ref_axis',(1.,0.,0.));
#8498=DIRECTION('center_axis',(9.61618982193066E-33,-1.03600583455278E-18,
-1.));
#8499=DIRECTION('ref_axis',(1.,0.,0.));
#8500=DIRECTION('',(0.,0.,-1.));
#8501=DIRECTION('center_axis',(-9.61618982193066E-33,1.03600583455278E-18,
1.));
#8502=DIRECTION('ref_axis',(1.,0.,0.));
#8503=DIRECTION('center_axis',(0.,0.,-1.));
#8504=DIRECTION('ref_axis',(1.,0.,0.));
#8505=DIRECTION('center_axis',(9.61618982193066E-33,-1.03600583455278E-18,
-1.));
#8506=DIRECTION('ref_axis',(1.,0.,0.));
#8507=DIRECTION('',(0.,0.,-1.));
#8508=DIRECTION('center_axis',(0.,0.,-1.));
#8509=DIRECTION('ref_axis',(1.,0.,0.));
#8510=DIRECTION('center_axis',(9.61618982193066E-33,-1.03600583455278E-18,
-1.));
#8511=DIRECTION('ref_axis',(1.,0.,0.));
#8512=DIRECTION('',(0.,0.,-1.));
#8513=DIRECTION('center_axis',(0.,0.,-1.));
#8514=DIRECTION('ref_axis',(1.,0.,0.));
#8515=DIRECTION('center_axis',(9.61618982193066E-33,-1.03600583455278E-18,
-1.));
#8516=DIRECTION('ref_axis',(1.,0.,0.));
#8517=DIRECTION('',(0.,0.,-1.));
#8518=DIRECTION('center_axis',(-9.61618982193066E-33,1.03600583455278E-18,
1.));
#8519=DIRECTION('ref_axis',(1.,0.,0.));
#8520=DIRECTION('center_axis',(0.86602540378444,0.499999999999998,0.));
#8521=DIRECTION('ref_axis',(0.499999999999998,-0.86602540378444,0.));
#8522=DIRECTION('',(0.499999999999998,-0.86602540378444,8.9720737119161E-19));
#8523=DIRECTION('',(0.,0.,-1.));
#8524=DIRECTION('',(0.499999999999998,-0.86602540378444,0.));
#8525=DIRECTION('',(0.,0.,-1.));
#8526=DIRECTION('center_axis',(1.60246890531964E-16,1.,0.));
#8527=DIRECTION('ref_axis',(1.,-1.60246890531964E-16,0.));
#8528=DIRECTION('',(1.,-1.60246890531964E-16,9.78220653549071E-33));
#8529=DIRECTION('',(0.,0.,-1.));
#8530=DIRECTION('',(1.,-1.60246890531964E-16,0.));
#8531=DIRECTION('center_axis',(-0.86602540378444,0.499999999999998,0.));
#8532=DIRECTION('ref_axis',(0.499999999999998,0.86602540378444,0.));
#8533=DIRECTION('',(0.499999999999998,0.86602540378444,-8.97207371191601E-19));
#8534=DIRECTION('',(0.,0.,-1.));
#8535=DIRECTION('',(0.499999999999998,0.86602540378444,0.));
#8536=DIRECTION('center_axis',(-0.86602540378444,-0.499999999999998,0.));
#8537=DIRECTION('ref_axis',(-0.499999999999998,0.86602540378444,0.));
#8538=DIRECTION('',(-0.499999999999998,0.86602540378444,-8.9720737119161E-19));
#8539=DIRECTION('',(0.,0.,-1.));
#8540=DIRECTION('',(-0.499999999999998,0.86602540378444,0.));
#8541=DIRECTION('center_axis',(-1.60246890531964E-16,-1.,0.));
#8542=DIRECTION('ref_axis',(-1.,1.60246890531964E-16,0.));
#8543=DIRECTION('',(-1.,1.60246890531964E-16,-9.78220653549071E-33));
#8544=DIRECTION('',(0.,0.,-1.));
#8545=DIRECTION('',(-1.,1.60246890531964E-16,0.));
#8546=DIRECTION('center_axis',(0.86602540378444,-0.499999999999998,0.));
#8547=DIRECTION('ref_axis',(-0.499999999999998,-0.86602540378444,0.));
#8548=DIRECTION('',(-0.499999999999998,-0.86602540378444,8.97207371191601E-19));
#8549=DIRECTION('',(-0.499999999999998,-0.86602540378444,0.));
#8550=DIRECTION('center_axis',(0.,0.,-1.));
#8551=DIRECTION('ref_axis',(-1.,0.,0.));
#8552=DIRECTION('center_axis',(0.,0.,1.));
#8553=DIRECTION('ref_axis',(1.,0.,0.));
#8554=DIRECTION('center_axis',(0.866025403784439,0.5,0.));
#8555=DIRECTION('ref_axis',(0.5,-0.866025403784439,0.));
#8556=DIRECTION('',(0.5,-0.866025403784439,8.97207371191609E-19));
#8557=DIRECTION('',(0.,0.,-1.));
#8558=DIRECTION('',(0.5,-0.866025403784439,0.));
#8559=DIRECTION('',(0.,0.,-1.));
#8560=DIRECTION('center_axis',(1.60246890531964E-16,1.,0.));
#8561=DIRECTION('ref_axis',(1.,-1.60246890531964E-16,0.));
#8562=DIRECTION('',(1.,-1.60246890531964E-16,9.78220653549071E-33));
#8563=DIRECTION('',(0.,0.,-1.));
#8564=DIRECTION('',(1.,-1.60246890531964E-16,0.));
#8565=DIRECTION('center_axis',(-0.866025403784438,0.5,0.));
#8566=DIRECTION('ref_axis',(0.5,0.866025403784438,0.));
#8567=DIRECTION('',(0.5,0.866025403784438,-8.97207371191599E-19));
#8568=DIRECTION('',(0.,0.,-1.));
#8569=DIRECTION('',(0.5,0.866025403784438,0.));
#8570=DIRECTION('center_axis',(-0.866025403784439,-0.499999999999999,0.));
#8571=DIRECTION('ref_axis',(-0.499999999999999,0.866025403784439,0.));
#8572=DIRECTION('',(-0.499999999999999,0.866025403784439,-8.97207371191609E-19));
#8573=DIRECTION('',(0.,0.,-1.));
#8574=DIRECTION('',(-0.499999999999999,0.866025403784439,0.));
#8575=DIRECTION('center_axis',(-1.60246890531964E-16,-1.,0.));
#8576=DIRECTION('ref_axis',(-1.,1.60246890531964E-16,0.));
#8577=DIRECTION('',(-1.,1.60246890531964E-16,-9.78220653549071E-33));
#8578=DIRECTION('',(0.,0.,-1.));
#8579=DIRECTION('',(-1.,1.60246890531964E-16,0.));
#8580=DIRECTION('center_axis',(0.866025403784439,-0.5,0.));
#8581=DIRECTION('ref_axis',(-0.5,-0.866025403784439,0.));
#8582=DIRECTION('',(-0.5,-0.866025403784439,8.97207371191599E-19));
#8583=DIRECTION('',(-0.5,-0.866025403784439,0.));
#8584=DIRECTION('center_axis',(0.,0.,-1.));
#8585=DIRECTION('ref_axis',(-1.,0.,0.));
#8586=DIRECTION('center_axis',(0.,0.,1.));
#8587=DIRECTION('ref_axis',(1.,0.,0.));
#8588=DIRECTION('center_axis',(0.,0.,-1.));
#8589=DIRECTION('ref_axis',(1.,0.,0.));
#8590=DIRECTION('',(0.,0.,-1.));
#8591=DIRECTION('center_axis',(0.,0.,1.));
#8592=DIRECTION('ref_axis',(1.,0.,0.));
#8593=DIRECTION('center_axis',(0.,0.,-1.));
#8594=DIRECTION('ref_axis',(1.,0.,0.));
#8595=DIRECTION('',(0.,0.,-1.));
#8596=DIRECTION('center_axis',(0.,0.,1.));
#8597=DIRECTION('ref_axis',(1.,0.,0.));
#8598=DIRECTION('center_axis',(0.,-1.,0.));
#8599=DIRECTION('ref_axis',(-1.,0.,0.));
#8600=DIRECTION('',(0.0523359562429438,0.,0.998629534754574));
#8601=DIRECTION('',(1.,0.,0.));
#8602=DIRECTION('',(-0.0523359562429438,0.,-0.998629534754574));
#8603=DIRECTION('',(1.,0.,0.));
#8604=DIRECTION('center_axis',(0.,-1.,0.));
#8605=DIRECTION('ref_axis',(-1.,0.,0.));
#8606=DIRECTION('',(0.,0.,-1.));
#8607=DIRECTION('',(1.,0.,0.));
#8608=DIRECTION('',(0.,0.,1.));
#8609=DIRECTION('',(1.,0.,0.));
#8610=DIRECTION('center_axis',(0.,-1.,0.));
#8611=DIRECTION('ref_axis',(-1.,0.,0.));
#8612=DIRECTION('',(0.,0.,-1.));
#8613=DIRECTION('',(1.,0.,0.));
#8614=DIRECTION('',(0.,0.,1.));
#8615=DIRECTION('',(1.,0.,0.));
#8616=DIRECTION('center_axis',(0.,-1.,0.));
#8617=DIRECTION('ref_axis',(-1.,0.,0.));
#8618=DIRECTION('',(0.,0.,-1.));
#8619=DIRECTION('',(1.,0.,0.));
#8620=DIRECTION('',(0.,0.,1.));
#8621=DIRECTION('',(1.,0.,0.));
#8622=DIRECTION('center_axis',(0.,1.,0.));
#8623=DIRECTION('ref_axis',(1.,0.,0.));
#8624=DIRECTION('',(-0.0523359562429438,0.,-0.998629534754574));
#8625=DIRECTION('',(-1.,0.,0.));
#8626=DIRECTION('',(0.0523359562429438,0.,0.998629534754574));
#8627=DIRECTION('',(-1.,0.,0.));
#8628=DIRECTION('center_axis',(0.,1.,0.));
#8629=DIRECTION('ref_axis',(1.,0.,0.));
#8630=DIRECTION('',(0.,0.,1.));
#8631=DIRECTION('',(-1.,0.,0.));
#8632=DIRECTION('',(0.,0.,-1.));
#8633=DIRECTION('',(-1.,0.,0.));
#8634=DIRECTION('center_axis',(0.,1.,0.));
#8635=DIRECTION('ref_axis',(1.,0.,0.));
#8636=DIRECTION('',(0.,0.,1.));
#8637=DIRECTION('',(-1.,0.,0.));
#8638=DIRECTION('',(0.,0.,-1.));
#8639=DIRECTION('',(-1.,0.,0.));
#8640=DIRECTION('center_axis',(0.,0.,1.));
#8641=DIRECTION('ref_axis',(1.,0.,0.));
#8642=DIRECTION('center_axis',(0.,0.,1.));
#8643=DIRECTION('ref_axis',(1.,0.,0.));
#8644=DIRECTION('center_axis',(0.,0.,1.));
#8645=DIRECTION('ref_axis',(1.,0.,0.));
#8646=DIRECTION('center_axis',(0.,0.,1.));
#8647=DIRECTION('ref_axis',(1.,0.,0.));
#8648=DIRECTION('center_axis',(0.,0.,1.));
#8649=DIRECTION('ref_axis',(1.,0.,0.));
#8650=DIRECTION('',(0.,1.,0.));
#8651=DIRECTION('',(0.,-1.,0.));
#8652=DIRECTION('center_axis',(0.,0.,1.));
#8653=DIRECTION('ref_axis',(1.,0.,0.));
#8654=DIRECTION('',(0.,-1.,0.));
#8655=DIRECTION('',(0.,1.,0.));
#8656=DIRECTION('center_axis',(0.,0.,1.));
#8657=DIRECTION('ref_axis',(1.,0.,0.));
#8658=DIRECTION('',(0.,-1.,0.));
#8659=DIRECTION('',(0.,1.,0.));
#8660=DIRECTION('center_axis',(0.,0.,1.));
#8661=DIRECTION('ref_axis',(1.,0.,0.));
#8662=DIRECTION('',(0.,-1.,0.));
#8663=DIRECTION('',(-1.,0.,0.));
#8664=DIRECTION('',(0.,1.,0.));
#8665=DIRECTION('center_axis',(0.,1.,0.));
#8666=DIRECTION('ref_axis',(1.,0.,0.));
#8667=DIRECTION('',(0.,0.,1.));
#8668=DIRECTION('',(-1.,0.,0.));
#8669=DIRECTION('',(0.,0.,-1.));
#8670=DIRECTION('center_axis',(-1.,0.,0.));
#8671=DIRECTION('ref_axis',(0.,-1.,0.));
#8672=DIRECTION('',(0.,-1.,0.));
#8673=DIRECTION('',(0.,-1.,1.03600583455278E-18));
#8674=DIRECTION('center_axis',(1.,0.,0.));
#8675=DIRECTION('ref_axis',(0.,1.,0.));
#8676=DIRECTION('',(0.,1.,0.));
#8677=DIRECTION('',(0.,1.,-1.03600583455278E-18));
#8678=DIRECTION('',(0.,1.,0.));
#8679=DIRECTION('center_axis',(1.,0.,0.));
#8680=DIRECTION('ref_axis',(0.,1.,0.));
#8681=DIRECTION('',(0.,1.,0.));
#8682=DIRECTION('',(0.,1.,-1.03600583455278E-18));
#8683=DIRECTION('',(0.,1.,0.));
#8684=DIRECTION('center_axis',(1.,0.,0.));
#8685=DIRECTION('ref_axis',(0.,1.,0.));
#8686=DIRECTION('',(0.,1.,0.));
#8687=DIRECTION('',(0.,1.,0.));
#8688=DIRECTION('center_axis',(0.998629534754574,0.,-0.0523359562429438));
#8689=DIRECTION('ref_axis',(-0.0523359562429438,0.,-0.998629534754574));
#8690=DIRECTION('',(0.,-1.,0.));
#8691=DIRECTION('',(5.42947651131849E-20,-1.,1.03600583455278E-18));
#8692=DIRECTION('',(0.,-1.,0.));
#8693=DIRECTION('center_axis',(0.,0.,1.));
#8694=DIRECTION('ref_axis',(1.,0.,0.));
#8695=DIRECTION('',(0.,-1.,0.));
#8696=DIRECTION('',(0.,-1.,0.));
#8697=DIRECTION('',(0.,-1.,0.));
#8698=DIRECTION('',(0.,1.,0.));
#8699=DIRECTION('',(0.,-1.,0.));
#8700=DIRECTION('',(0.,1.,0.));
#8701=DIRECTION('',(0.,-1.,0.));
#8702=DIRECTION('',(0.,-1.,0.));
#8703=DIRECTION('',(0.,-1.,0.));
#8704=DIRECTION('',(0.,1.,0.));
#8705=DIRECTION('',(0.,1.,0.));
#8706=DIRECTION('center_axis',(0.,0.,1.));
#8707=DIRECTION('ref_axis',(1.,0.,0.));
#8708=DIRECTION('center_axis',(-9.61618982193066E-33,1.03600583455278E-18,
1.));
#8709=DIRECTION('ref_axis',(1.,0.,0.));
#8710=DIRECTION('',(0.,0.,-1.));
#8711=DIRECTION('center_axis',(0.,0.,1.));
#8712=DIRECTION('ref_axis',(1.,0.,0.));
#8713=DIRECTION('',(0.,0.,-1.));
#8714=DIRECTION('center_axis',(1.,0.,0.));
#8715=DIRECTION('ref_axis',(0.,1.,0.));
#8716=DIRECTION('',(0.,1.,-1.03600583455278E-18));
#8717=DIRECTION('center_axis',(0.994044372876412,-0.108976074221552,-1.1933167131821E-14));
#8718=DIRECTION('ref_axis',(-0.108857570442347,-0.992963419871597,0.0466226999892957));
#8719=DIRECTION('center_axis',(-9.61618982193066E-33,1.03600583455278E-18,
1.));
#8720=DIRECTION('ref_axis',(1.,0.,9.61618982193066E-33));
#8721=DIRECTION('center_axis',(-9.61618982193066E-33,1.03600583455278E-18,
1.));
#8722=DIRECTION('ref_axis',(1.,0.,9.61618982193066E-33));
#8723=DIRECTION('',(-5.42947651131849E-20,-1.,1.03600583455278E-18));
#8724=DIRECTION('center_axis',(-1.,0.,0.));
#8725=DIRECTION('ref_axis',(0.,-1.,0.));
#8726=DIRECTION('',(0.,-1.,1.03600583455278E-18));
#8727=DIRECTION('center_axis',(-9.61618982193066E-33,1.03600583455278E-18,
1.));
#8728=DIRECTION('ref_axis',(1.,0.,9.61618982193066E-33));
#8729=DIRECTION('center_axis',(-1.,0.,0.));
#8730=DIRECTION('ref_axis',(0.,-1.,0.));
#8731=DIRECTION('center_axis',(-1.,0.,0.));
#8732=DIRECTION('ref_axis',(0.,-1.,0.));
#8733=DIRECTION('',(0.,-1.,1.03600583455278E-18));
#8734=DIRECTION('center_axis',(-0.999738255753194,0.0228783737088345,0.));
#8735=DIRECTION('ref_axis',(0.,0.,1.));
#8736=DIRECTION('center_axis',(-9.61618982193066E-33,1.03600583455278E-18,
1.));
#8737=DIRECTION('ref_axis',(1.,0.,9.61618982193066E-33));
#8738=DIRECTION('',(-5.42947651131849E-20,1.,-1.03600583455278E-18));
#8739=DIRECTION('center_axis',(-0.999738255790058,-0.0228783720979604,1.69987959829136E-9));
#8740=DIRECTION('ref_axis',(-0.022845652001536,0.998308458201847,0.0534630570326489));
#8741=DIRECTION('center_axis',(-0.375013085256251,-0.833398400631247,0.405970801550885));
#8742=DIRECTION('ref_axis',(-0.565498005067694,0.552672693214782,0.612180447612612));
#8743=DIRECTION('center_axis',(-7.78474640228738E-11,1.,0.));
#8744=DIRECTION('ref_axis',(0.,0.,1.));
#8745=DIRECTION('center_axis',(0.0522645732252412,-0.0522112666801462,0.997267465636596));
#8746=DIRECTION('ref_axis',(-0.998629534754574,0.,0.0523359562429445));
#8747=DIRECTION('center_axis',(0.361627795167438,-0.818371417997736,0.44664701943113));
#8748=DIRECTION('ref_axis',(0.514966362801186,0.574689674697898,0.636035708886648));
#8749=DIRECTION('center_axis',(0.994044372876412,0.108976074221546,-5.96658356591051E-15));
#8750=DIRECTION('ref_axis',(5.9211894646675E-15,7.40148683083438E-16,1.));
#8751=DIRECTION('center_axis',(-0.052263633556273,-0.0525535553916586,0.997249535684621));
#8752=DIRECTION('ref_axis',(-0.108857570442347,0.992963419871597,0.0466226999892949));
#8753=DIRECTION('center_axis',(0.,1.,0.));
#8754=DIRECTION('ref_axis',(0.998629534754574,0.,0.0523359562429438));
#8755=DIRECTION('center_axis',(0.375013085403515,-0.833398400816333,-0.405970801034895));
#8756=DIRECTION('ref_axis',(-0.565498005700927,-0.552672692935682,0.612180447279637));
#8757=DIRECTION('center_axis',(0.0522645732252408,0.0522112666801459,0.997267465636596));
#8758=DIRECTION('ref_axis',(-0.0228456520015352,-0.998308458201847,0.0534630570326489));
#8759=DIRECTION('center_axis',(-4.07418268117644E-12,-1.,-7.77400366303027E-11));
#8760=DIRECTION('ref_axis',(-0.998629534754574,0.,0.0523359562429438));
#8761=DIRECTION('center_axis',(-5.42947651131849E-20,1.,-1.03600583455278E-18));
#8762=DIRECTION('ref_axis',(-0.688354575693754,0.,0.725374371012288));
#8763=DIRECTION('center_axis',(-0.361627795167436,-0.818371417997736,-0.446647019431131));
#8764=DIRECTION('ref_axis',(0.514966362801185,-0.574689674697896,0.636035708886651));
#8765=DIRECTION('center_axis',(-0.0522636335562752,0.0525535553916633,0.99724953568462));
#8766=DIRECTION('ref_axis',(0.998629534754574,0.,0.0523359562429442));
#8767=DIRECTION('center_axis',(0.,-1.,0.));
#8768=DIRECTION('ref_axis',(0.,0.,1.));
#8769=DIRECTION('center_axis',(-5.42947651131849E-20,-1.,1.03600583455278E-18));
#8770=DIRECTION('ref_axis',(0.688354575693754,0.,0.725374371012288));
#8771=DIRECTION('',(5.42947651131849E-20,1.,-1.03600583455278E-18));
#8772=DIRECTION('center_axis',(-0.998629534754574,0.,-0.0523359562429438));
#8773=DIRECTION('ref_axis',(-0.0523359562429438,0.,0.998629534754574));
#8774=DIRECTION('center_axis',(-0.375013085256251,-0.833398400631247,0.405970801550885));
#8775=DIRECTION('ref_axis',(-0.565498005067695,0.552672693214781,0.612180447612612));
#8776=DIRECTION('center_axis',(-7.78474640228738E-11,1.,0.));
#8777=DIRECTION('ref_axis',(0.,0.,1.));
#8778=DIRECTION('center_axis',(-0.999738255790058,-0.0228783720979604,1.69987959829136E-9));
#8779=DIRECTION('ref_axis',(-0.022845652001536,0.998308458201847,0.0534630570326489));
#8780=DIRECTION('center_axis',(0.0522645732252412,-0.0522112666801462,0.997267465636596));
#8781=DIRECTION('ref_axis',(-0.998629534754574,0.,0.0523359562429445));
#8782=DIRECTION('center_axis',(0.361627795167442,-0.818371417997735,0.446647019431129));
#8783=DIRECTION('ref_axis',(0.514966362801186,0.574689674697898,0.636035708886649));
#8784=DIRECTION('center_axis',(0.994044372876412,0.108976074221546,-5.96658356591051E-15));
#8785=DIRECTION('ref_axis',(5.9211894646675E-15,7.40148683083438E-16,1.));
#8786=DIRECTION('center_axis',(0.,1.,0.));
#8787=DIRECTION('ref_axis',(0.998629534754574,0.,0.0523359562429438));
#8788=DIRECTION('center_axis',(-0.052263633556273,-0.0525535553916586,0.997249535684621));
#8789=DIRECTION('ref_axis',(-0.108857570442347,0.992963419871597,0.0466226999892949));
#8790=DIRECTION('center_axis',(0.375013085403515,-0.833398400816333,-0.405970801034895));
#8791=DIRECTION('ref_axis',(-0.565498005700926,-0.552672692935682,0.612180447279637));
#8792=DIRECTION('center_axis',(-0.999738255753194,0.0228783737088345,0.));
#8793=DIRECTION('ref_axis',(0.,0.,1.));
#8794=DIRECTION('center_axis',(-4.07418268117644E-12,-1.,-7.77400366303027E-11));
#8795=DIRECTION('ref_axis',(-0.998629534754574,0.,0.0523359562429438));
#8796=DIRECTION('center_axis',(0.0522645732252408,0.0522112666801459,0.997267465636596));
#8797=DIRECTION('ref_axis',(-0.0228456520015352,-0.998308458201847,0.0534630570326489));
#8798=DIRECTION('center_axis',(-5.42947651131849E-20,1.,-1.03600583455278E-18));
#8799=DIRECTION('ref_axis',(-0.688354575693754,0.,0.725374371012288));
#8800=DIRECTION('',(5.42947651131849E-20,-1.,1.03600583455278E-18));
#8801=DIRECTION('',(-5.42947651131849E-20,1.,-1.03600583455278E-18));
#8802=DIRECTION('center_axis',(-0.361627795167436,-0.818371417997736,-0.446647019431131));
#8803=DIRECTION('ref_axis',(0.51496636280118,-0.574689674697898,0.636035708886653));
#8804=DIRECTION('center_axis',(-0.0522636335562752,0.0525535553916633,0.99724953568462));
#8805=DIRECTION('ref_axis',(0.998629534754574,0.,0.0523359562429441));
#8806=DIRECTION('center_axis',(0.,-1.,0.));
#8807=DIRECTION('ref_axis',(0.,0.,1.));
#8808=DIRECTION('center_axis',(0.994044372876412,-0.108976074221552,-1.1933167131821E-14));
#8809=DIRECTION('ref_axis',(-0.108857570442347,-0.992963419871597,0.0466226999892957));
#8810=DIRECTION('center_axis',(-5.42947651131849E-20,-1.,1.03600583455278E-18));
#8811=DIRECTION('ref_axis',(0.688354575693754,0.,0.725374371012288));
#8812=DIRECTION('',(5.42947651131849E-20,1.,-1.03600583455278E-18));
#8813=DIRECTION('',(-5.42947651131849E-20,-1.,1.03600583455278E-18));
#8814=DIRECTION('center_axis',(0.998629534754574,0.,-0.0523359562429438));
#8815=DIRECTION('ref_axis',(-0.0523359562429438,0.,-0.998629534754574));
#8816=DIRECTION('center_axis',(-9.61618982193066E-33,1.03600583455278E-18,
1.));
#8817=DIRECTION('ref_axis',(1.,0.,9.61618982193066E-33));
#8818=DIRECTION('center_axis',(-0.998629534754574,0.,-0.0523359562429438));
#8819=DIRECTION('ref_axis',(-0.0523359562429438,0.,0.998629534754574));
#8820=DIRECTION('axis',(0.,0.,1.));
#8821=DIRECTION('refdir',(1.,0.,0.));
#8822=DIRECTION('center_axis',(0.,0.,-1.));
#8823=DIRECTION('ref_axis',(1.,0.,0.));
#8824=DIRECTION('center_axis',(-6.04309184969008E-32,-6.38489691472444E-32,
-1.));
#8825=DIRECTION('ref_axis',(1.,0.,0.));
#8826=DIRECTION('',(0.,0.,-1.));
#8827=DIRECTION('center_axis',(1.44549646912992E-31,1.50240180416177E-18,
1.));
#8828=DIRECTION('ref_axis',(1.,0.,0.));
#8829=DIRECTION('center_axis',(0.,0.,-1.));
#8830=DIRECTION('ref_axis',(1.,0.,0.));
#8831=DIRECTION('center_axis',(-6.04309184969008E-32,-6.38489691472444E-32,
-1.));
#8832=DIRECTION('ref_axis',(1.,0.,0.));
#8833=DIRECTION('',(0.,0.,-1.));
#8834=DIRECTION('center_axis',(1.44549646912992E-31,1.50240180416177E-18,
1.));
#8835=DIRECTION('ref_axis',(1.,0.,0.));
#8836=DIRECTION('center_axis',(0.,0.,1.));
#8837=DIRECTION('ref_axis',(1.,0.,0.));
#8838=DIRECTION('center_axis',(0.,0.,1.));
#8839=DIRECTION('ref_axis',(1.,0.,0.));
#8840=DIRECTION('center_axis',(0.,0.,-1.));
#8841=DIRECTION('ref_axis',(1.,0.,0.));
#8842=DIRECTION('center_axis',(0.,0.,-1.));
#8843=DIRECTION('ref_axis',(1.,0.,0.));
#8844=DIRECTION('center_axis',(0.,0.,-1.));
#8845=DIRECTION('ref_axis',(1.,0.,0.));
#8846=DIRECTION('',(0.,0.,1.));
#8847=DIRECTION('center_axis',(0.,0.,1.));
#8848=DIRECTION('ref_axis',(1.,0.,0.));
#8849=DIRECTION('center_axis',(0.,0.,1.));
#8850=DIRECTION('ref_axis',(1.,0.,0.));
#8851=DIRECTION('center_axis',(0.,0.,1.));
#8852=DIRECTION('ref_axis',(1.,0.,0.));
#8853=DIRECTION('center_axis',(0.,0.,-1.));
#8854=DIRECTION('ref_axis',(1.,0.,0.));
#8855=DIRECTION('center_axis',(0.,0.,-1.));
#8856=DIRECTION('ref_axis',(1.,0.,0.));
#8857=DIRECTION('center_axis',(0.,0.,-1.));
#8858=DIRECTION('ref_axis',(1.,0.,0.));
#8859=DIRECTION('',(0.,0.,1.));
#8860=DIRECTION('center_axis',(0.,0.,1.));
#8861=DIRECTION('ref_axis',(1.,0.,0.));
#8862=DIRECTION('center_axis',(0.,0.,1.));
#8863=DIRECTION('ref_axis',(1.,0.,0.));
#8864=DIRECTION('center_axis',(0.,0.,1.));
#8865=DIRECTION('ref_axis',(1.,0.,0.));
#8866=DIRECTION('center_axis',(0.,0.,-1.));
#8867=DIRECTION('ref_axis',(1.,0.,0.));
#8868=DIRECTION('center_axis',(0.,0.,-1.));
#8869=DIRECTION('ref_axis',(1.,0.,0.));
#8870=DIRECTION('center_axis',(0.,0.,-1.));
#8871=DIRECTION('ref_axis',(1.,0.,0.));
#8872=DIRECTION('',(0.,0.,1.));
#8873=DIRECTION('center_axis',(0.,0.,1.));
#8874=DIRECTION('ref_axis',(1.,0.,0.));
#8875=DIRECTION('center_axis',(0.,0.,1.));
#8876=DIRECTION('ref_axis',(1.,0.,0.));
#8877=DIRECTION('center_axis',(0.,0.,1.));
#8878=DIRECTION('ref_axis',(1.,0.,0.));
#8879=DIRECTION('center_axis',(0.,0.,-1.));
#8880=DIRECTION('ref_axis',(1.,0.,0.));
#8881=DIRECTION('center_axis',(0.,0.,-1.));
#8882=DIRECTION('ref_axis',(1.,0.,0.));
#8883=DIRECTION('center_axis',(0.,0.,-1.));
#8884=DIRECTION('ref_axis',(1.,0.,0.));
#8885=DIRECTION('',(0.,0.,1.));
#8886=DIRECTION('center_axis',(0.,0.,1.));
#8887=DIRECTION('ref_axis',(1.,0.,0.));
#8888=DIRECTION('center_axis',(0.,0.,-1.));
#8889=DIRECTION('ref_axis',(1.,0.,0.));
#8890=DIRECTION('',(0.,0.,1.));
#8891=DIRECTION('center_axis',(1.44549646912992E-31,1.50240180416177E-18,
1.));
#8892=DIRECTION('ref_axis',(1.,0.,0.));
#8893=DIRECTION('center_axis',(0.,0.,-1.));
#8894=DIRECTION('ref_axis',(1.,0.,0.));
#8895=DIRECTION('',(0.,0.,1.));
#8896=DIRECTION('center_axis',(1.44549646912992E-31,1.50240180416177E-18,
1.));
#8897=DIRECTION('ref_axis',(1.,0.,0.));
#8898=DIRECTION('center_axis',(0.,0.,-1.));
#8899=DIRECTION('ref_axis',(1.,0.,0.));
#8900=DIRECTION('',(0.,0.,1.));
#8901=DIRECTION('center_axis',(1.44549646912992E-31,1.50240180416177E-18,
1.));
#8902=DIRECTION('ref_axis',(1.,0.,0.));
#8903=DIRECTION('center_axis',(0.,0.,-1.));
#8904=DIRECTION('ref_axis',(1.,0.,0.));
#8905=DIRECTION('',(0.,0.,1.));
#8906=DIRECTION('center_axis',(1.44549646912992E-31,1.50240180416177E-18,
1.));
#8907=DIRECTION('ref_axis',(1.,0.,0.));
#8908=DIRECTION('center_axis',(0.,1.,0.));
#8909=DIRECTION('ref_axis',(0.,0.,1.));
#8910=DIRECTION('center_axis',(0.993165917563083,0.116711011438853,0.));
#8911=DIRECTION('ref_axis',(-0.116587207627638,0.992112394641407,0.0460480120795941));
#8912=DIRECTION('center_axis',(-3.34618268251883E-33,-1.,6.38489691472444E-32));
#8913=DIRECTION('ref_axis',(0.688354575693762,0.,0.72537437101228));
#8914=DIRECTION('center_axis',(0.,1.,0.));
#8915=DIRECTION('ref_axis',(0.,0.,1.));
#8916=DIRECTION('',(3.34618268251883E-33,1.,-6.38489691472444E-32));
#8917=DIRECTION('',(-3.34618268251883E-33,-1.,6.38489691472444E-32));
#8918=DIRECTION('center_axis',(0.993165917563077,-0.116711011438899,0.));
#8919=DIRECTION('ref_axis',(0.,0.,1.));
#8920=DIRECTION('center_axis',(0.999711469489423,-0.0240203615980049,0.));
#8921=DIRECTION('ref_axis',(0.,0.,1.));
#8922=DIRECTION('center_axis',(-3.69655756055634E-12,-1.,2.05200165779092E-26));
#8923=DIRECTION('ref_axis',(5.55111512312576E-15,0.,1.));
#8924=DIRECTION('center_axis',(-3.3461826825185E-33,1.,-6.38489691472444E-32));
#8925=DIRECTION('ref_axis',(-0.688354575693751,0.,0.72537437101229));
#8926=DIRECTION('center_axis',(0.,-1.,0.));
#8927=DIRECTION('ref_axis',(0.,0.,1.));
#8928=DIRECTION('',(3.3461826825185E-33,-1.,6.38489691472444E-32));
#8929=DIRECTION('',(-3.3461826825185E-33,1.,-6.38489691472444E-32));
#8930=DIRECTION('center_axis',(-0.999711469481833,-0.0240203619138888,2.77475672850144E-15));
#8931=DIRECTION('ref_axis',(2.77555756156288E-15,0.,1.));
#8932=DIRECTION('center_axis',(0.998629534754574,0.,-0.0523359562429439));
#8933=DIRECTION('ref_axis',(-0.0523359562429439,0.,-0.998629534754574));
#8934=DIRECTION('',(0.,1.,0.));
#8935=DIRECTION('center_axis',(6.04309184969008E-32,6.38489691472444E-32,
1.));
#8936=DIRECTION('ref_axis',(1.,0.,-6.04309184969008E-32));
#8937=DIRECTION('center_axis',(-0.998629534754574,0.,-0.0523359562429491));
#8938=DIRECTION('ref_axis',(-0.0523359562429491,0.,0.998629534754574));
#8939=DIRECTION('',(0.,-1.,0.));
#8940=DIRECTION('center_axis',(1.44549646912992E-31,1.50240180416177E-18,
1.));
#8941=DIRECTION('ref_axis',(1.,0.,-1.44549646912992E-31));
#8942=DIRECTION('axis',(0.,0.,1.));
#8943=DIRECTION('refdir',(1.,0.,0.));
#8944=DIRECTION('center_axis',(0.,0.,1.));
#8945=DIRECTION('ref_axis',(1.,0.,0.));
#8946=DIRECTION('',(0.,0.,-1.));
#8947=DIRECTION('center_axis',(0.,0.,-1.));
#8948=DIRECTION('ref_axis',(1.,0.,0.));
#8949=DIRECTION('center_axis',(0.,0.,1.));
#8950=DIRECTION('ref_axis',(1.,0.,0.));
#8951=DIRECTION('',(0.,0.,-1.));
#8952=DIRECTION('center_axis',(0.,0.,1.));
#8953=DIRECTION('ref_axis',(1.,0.,0.));
#8954=DIRECTION('',(0.,0.,-1.));
#8955=DIRECTION('center_axis',(0.,0.,1.));
#8956=DIRECTION('ref_axis',(1.,0.,0.));
#8957=DIRECTION('',(0.,0.,-1.));
#8958=DIRECTION('center_axis',(0.,0.,1.));
#8959=DIRECTION('ref_axis',(1.,0.,0.));
#8960=DIRECTION('',(0.,0.,-1.));
#8961=DIRECTION('center_axis',(0.,0.,1.));
#8962=DIRECTION('ref_axis',(1.,0.,0.));
#8963=DIRECTION('',(0.,0.,-1.));
#8964=DIRECTION('center_axis',(0.,0.,1.));
#8965=DIRECTION('ref_axis',(1.,0.,0.));
#8966=DIRECTION('',(0.,0.,-1.));
#8967=DIRECTION('center_axis',(0.,0.,1.));
#8968=DIRECTION('ref_axis',(1.,0.,0.));
#8969=DIRECTION('',(0.,0.,-1.));
#8970=DIRECTION('center_axis',(0.,0.,1.));
#8971=DIRECTION('ref_axis',(1.,0.,0.));
#8972=DIRECTION('',(0.,0.,-1.));
#8973=DIRECTION('center_axis',(0.,0.,1.));
#8974=DIRECTION('ref_axis',(1.,0.,0.));
#8975=DIRECTION('',(0.,0.,-1.));
#8976=DIRECTION('center_axis',(0.,0.,1.));
#8977=DIRECTION('ref_axis',(1.,0.,0.));
#8978=DIRECTION('',(0.,0.,-1.));
#8979=DIRECTION('center_axis',(0.,0.,1.));
#8980=DIRECTION('ref_axis',(1.,0.,0.));
#8981=DIRECTION('',(0.,0.,-1.));
#8982=DIRECTION('center_axis',(0.,0.,1.));
#8983=DIRECTION('ref_axis',(1.,0.,0.));
#8984=DIRECTION('',(0.,0.,-1.));
#8985=DIRECTION('center_axis',(0.,0.,1.));
#8986=DIRECTION('ref_axis',(1.,0.,0.));
#8987=DIRECTION('',(0.,0.,-1.));
#8988=DIRECTION('center_axis',(0.,0.,1.));
#8989=DIRECTION('ref_axis',(1.,0.,0.));
#8990=DIRECTION('',(0.,0.,-1.));
#8991=DIRECTION('center_axis',(0.,0.,1.));
#8992=DIRECTION('ref_axis',(1.,0.,0.));
#8993=DIRECTION('',(0.,0.,-1.));
#8994=DIRECTION('center_axis',(0.,0.,1.));
#8995=DIRECTION('ref_axis',(1.,0.,0.));
#8996=DIRECTION('',(0.,0.,-1.));
#8997=DIRECTION('center_axis',(0.,0.,1.));
#8998=DIRECTION('ref_axis',(1.,0.,0.));
#8999=DIRECTION('',(0.,0.,-1.));
#9000=DIRECTION('center_axis',(0.,0.,1.));
#9001=DIRECTION('ref_axis',(1.,0.,0.));
#9002=DIRECTION('',(0.,0.,-1.));
#9003=DIRECTION('center_axis',(0.,0.,1.));
#9004=DIRECTION('ref_axis',(1.,0.,0.));
#9005=DIRECTION('',(0.,0.,-1.));
#9006=DIRECTION('center_axis',(0.,0.,1.));
#9007=DIRECTION('ref_axis',(1.,0.,0.));
#9008=DIRECTION('',(0.,0.,-1.));
#9009=DIRECTION('center_axis',(0.,0.,1.));
#9010=DIRECTION('ref_axis',(1.,0.,0.));
#9011=DIRECTION('',(0.,0.,-1.));
#9012=DIRECTION('center_axis',(0.,0.,1.));
#9013=DIRECTION('ref_axis',(1.,0.,0.));
#9014=DIRECTION('',(0.,0.,-1.));
#9015=DIRECTION('center_axis',(0.,0.,1.));
#9016=DIRECTION('ref_axis',(1.,0.,0.));
#9017=DIRECTION('',(0.,0.,-1.));
#9018=DIRECTION('center_axis',(0.,0.,1.));
#9019=DIRECTION('ref_axis',(1.,0.,0.));
#9020=DIRECTION('',(0.,0.,-1.));
#9021=DIRECTION('center_axis',(0.,0.,1.));
#9022=DIRECTION('ref_axis',(1.,0.,0.));
#9023=DIRECTION('',(0.,0.,-1.));
#9024=DIRECTION('center_axis',(0.,0.,1.));
#9025=DIRECTION('ref_axis',(1.,0.,0.));
#9026=DIRECTION('',(0.,0.,-1.));
#9027=DIRECTION('center_axis',(0.,0.,1.));
#9028=DIRECTION('ref_axis',(1.,0.,0.));
#9029=DIRECTION('',(0.,0.,-1.));
#9030=DIRECTION('center_axis',(0.,0.,1.));
#9031=DIRECTION('ref_axis',(1.,0.,0.));
#9032=DIRECTION('',(0.,0.,-1.));
#9033=DIRECTION('center_axis',(0.,0.,1.));
#9034=DIRECTION('ref_axis',(1.,0.,0.));
#9035=DIRECTION('',(0.,0.,-1.));
#9036=DIRECTION('center_axis',(0.,0.,1.));
#9037=DIRECTION('ref_axis',(1.,-2.42503376499884E-13,0.));
#9038=DIRECTION('',(0.,0.,1.));
#9039=DIRECTION('center_axis',(0.,0.,-1.));
#9040=DIRECTION('ref_axis',(1.,-2.42503376499884E-13,0.));
#9041=DIRECTION('center_axis',(0.,0.,1.));
#9042=DIRECTION('ref_axis',(1.,-2.42503376499884E-13,0.));
#9043=DIRECTION('',(0.,0.,1.));
#9044=DIRECTION('center_axis',(0.,0.,1.));
#9045=DIRECTION('ref_axis',(1.,-2.42503376499884E-13,0.));
#9046=DIRECTION('',(0.,0.,1.));
#9047=DIRECTION('center_axis',(0.,0.,1.));
#9048=DIRECTION('ref_axis',(1.,-2.42503376499884E-13,0.));
#9049=DIRECTION('',(0.,0.,1.));
#9050=DIRECTION('center_axis',(0.,0.,1.));
#9051=DIRECTION('ref_axis',(1.,-2.42503376499884E-13,0.));
#9052=DIRECTION('',(0.,0.,1.));
#9053=DIRECTION('center_axis',(0.,0.,1.));
#9054=DIRECTION('ref_axis',(1.,-2.42503376499884E-13,0.));
#9055=DIRECTION('',(0.,0.,1.));
#9056=DIRECTION('center_axis',(0.,0.,1.));
#9057=DIRECTION('ref_axis',(1.,-2.42503376499884E-13,0.));
#9058=DIRECTION('',(0.,0.,1.));
#9059=DIRECTION('center_axis',(0.,0.,1.));
#9060=DIRECTION('ref_axis',(1.,-2.42503376499884E-13,0.));
#9061=DIRECTION('',(0.,0.,1.));
#9062=DIRECTION('center_axis',(0.,0.,1.));
#9063=DIRECTION('ref_axis',(1.,-2.42503376499884E-13,0.));
#9064=DIRECTION('',(0.,0.,1.));
#9065=DIRECTION('center_axis',(0.,0.,1.));
#9066=DIRECTION('ref_axis',(1.,-2.42503376499884E-13,0.));
#9067=DIRECTION('',(0.,0.,1.));
#9068=DIRECTION('center_axis',(0.,0.,1.));
#9069=DIRECTION('ref_axis',(1.,-2.42503376499884E-13,0.));
#9070=DIRECTION('',(0.,0.,1.));
#9071=DIRECTION('center_axis',(0.,0.,1.));
#9072=DIRECTION('ref_axis',(1.,-2.42503376499884E-13,0.));
#9073=DIRECTION('',(0.,0.,1.));
#9074=DIRECTION('center_axis',(0.,0.,1.));
#9075=DIRECTION('ref_axis',(1.,-2.42503376499884E-13,0.));
#9076=DIRECTION('',(0.,0.,1.));
#9077=DIRECTION('center_axis',(0.,0.,1.));
#9078=DIRECTION('ref_axis',(1.,-2.42503376499884E-13,0.));
#9079=DIRECTION('',(0.,0.,1.));
#9080=DIRECTION('center_axis',(0.,0.,1.));
#9081=DIRECTION('ref_axis',(1.,-2.42503376499884E-13,0.));
#9082=DIRECTION('',(0.,0.,1.));
#9083=DIRECTION('center_axis',(0.,0.,1.));
#9084=DIRECTION('ref_axis',(1.,-2.42503376499884E-13,0.));
#9085=DIRECTION('',(0.,0.,1.));
#9086=DIRECTION('center_axis',(0.,0.,1.));
#9087=DIRECTION('ref_axis',(1.,-2.42503376499884E-13,0.));
#9088=DIRECTION('',(0.,0.,1.));
#9089=DIRECTION('center_axis',(0.,0.,1.));
#9090=DIRECTION('ref_axis',(1.,-2.42503376499884E-13,0.));
#9091=DIRECTION('',(0.,0.,1.));
#9092=DIRECTION('center_axis',(0.,0.,1.));
#9093=DIRECTION('ref_axis',(1.,-2.42503376499884E-13,0.));
#9094=DIRECTION('',(0.,0.,1.));
#9095=DIRECTION('center_axis',(0.,0.,1.));
#9096=DIRECTION('ref_axis',(1.,-2.42503376499884E-13,0.));
#9097=DIRECTION('',(0.,0.,1.));
#9098=DIRECTION('center_axis',(0.,0.,1.));
#9099=DIRECTION('ref_axis',(1.,-2.42503376499884E-13,0.));
#9100=DIRECTION('',(0.,0.,1.));
#9101=DIRECTION('center_axis',(0.,0.,1.));
#9102=DIRECTION('ref_axis',(1.,-2.42503376499884E-13,0.));
#9103=DIRECTION('',(0.,0.,1.));
#9104=DIRECTION('center_axis',(0.,0.,1.));
#9105=DIRECTION('ref_axis',(1.,-2.42503376499884E-13,0.));
#9106=DIRECTION('',(0.,0.,1.));
#9107=DIRECTION('center_axis',(0.,0.,1.));
#9108=DIRECTION('ref_axis',(1.,-2.42503376499884E-13,0.));
#9109=DIRECTION('',(0.,0.,1.));
#9110=DIRECTION('center_axis',(0.,0.,1.));
#9111=DIRECTION('ref_axis',(1.,-2.42503376499884E-13,0.));
#9112=DIRECTION('',(0.,0.,1.));
#9113=DIRECTION('center_axis',(0.,0.,1.));
#9114=DIRECTION('ref_axis',(1.,-2.42503376499884E-13,0.));
#9115=DIRECTION('',(0.,0.,1.));
#9116=DIRECTION('center_axis',(0.,0.,1.));
#9117=DIRECTION('ref_axis',(1.,-2.42503376499884E-13,0.));
#9118=DIRECTION('',(0.,0.,1.));
#9119=DIRECTION('center_axis',(0.,0.,1.));
#9120=DIRECTION('ref_axis',(1.,-2.42503376499884E-13,0.));
#9121=DIRECTION('',(0.,0.,1.));
#9122=DIRECTION('center_axis',(0.,0.,1.));
#9123=DIRECTION('ref_axis',(1.,-2.42503376499884E-13,0.));
#9124=DIRECTION('',(0.,0.,1.));
#9125=DIRECTION('center_axis',(0.,0.,1.));
#9126=DIRECTION('ref_axis',(1.,-2.42503376499884E-13,0.));
#9127=DIRECTION('',(0.,0.,1.));
#9128=DIRECTION('center_axis',(0.,0.,-1.));
#9129=DIRECTION('ref_axis',(1.,0.,0.));
#9130=DIRECTION('center_axis',(0.,0.,-1.));
#9131=DIRECTION('ref_axis',(1.,0.,0.));
#9132=DIRECTION('',(0.707106781186547,8.65956056235493E-17,0.707106781186548));
#9133=DIRECTION('center_axis',(0.,0.,1.));
#9134=DIRECTION('ref_axis',(1.,0.,0.));
#9135=DIRECTION('center_axis',(0.,0.,1.));
#9136=DIRECTION('ref_axis',(1.,-2.42503376499884E-13,0.));
#9137=DIRECTION('center_axis',(0.,0.,-1.));
#9138=DIRECTION('ref_axis',(1.,-2.42503376499884E-13,0.));
#9139=DIRECTION('center_axis',(0.,0.,1.));
#9140=DIRECTION('ref_axis',(1.,0.,0.));
#9141=DIRECTION('center_axis',(-1.92296268638356E-16,-1.,0.));
#9142=DIRECTION('ref_axis',(1.,-1.92296268638356E-16,0.));
#9143=DIRECTION('',(1.,-1.92296268638356E-16,0.));
#9144=DIRECTION('',(0.,0.,1.));
#9145=DIRECTION('',(1.,-1.92296268638356E-16,0.));
#9146=DIRECTION('',(0.,0.,1.));
#9147=DIRECTION('center_axis',(-0.866025403784439,-0.5,0.));
#9148=DIRECTION('ref_axis',(0.5,-0.866025403784439,0.));
#9149=DIRECTION('',(0.5,-0.866025403784439,0.));
#9150=DIRECTION('',(0.,0.,1.));
#9151=DIRECTION('',(0.5,-0.866025403784439,0.));
#9152=DIRECTION('center_axis',(-0.866025403784439,0.5,0.));
#9153=DIRECTION('ref_axis',(-0.5,-0.866025403784439,0.));
#9154=DIRECTION('',(-0.5,-0.866025403784439,0.));
#9155=DIRECTION('',(0.,0.,1.));
#9156=DIRECTION('',(-0.5,-0.866025403784438,0.));
#9157=DIRECTION('center_axis',(1.92296268638356E-16,1.,0.));
#9158=DIRECTION('ref_axis',(-1.,1.92296268638356E-16,0.));
#9159=DIRECTION('',(-1.,1.92296268638356E-16,0.));
#9160=DIRECTION('',(0.,0.,1.));
#9161=DIRECTION('',(-1.,1.92296268638356E-16,0.));
#9162=DIRECTION('center_axis',(0.866025403784439,0.5,0.));
#9163=DIRECTION('ref_axis',(-0.5,0.866025403784439,0.));
#9164=DIRECTION('',(-0.5,0.866025403784439,0.));
#9165=DIRECTION('',(0.,0.,1.));
#9166=DIRECTION('',(-0.5,0.866025403784439,0.));
#9167=DIRECTION('center_axis',(0.866025403784439,-0.5,0.));
#9168=DIRECTION('ref_axis',(0.5,0.866025403784439,0.));
#9169=DIRECTION('',(0.5,0.866025403784439,0.));
#9170=DIRECTION('',(0.5,0.866025403784439,0.));
#9171=DIRECTION('center_axis',(0.,0.,1.));
#9172=DIRECTION('ref_axis',(1.,0.,0.));
#9173=DIRECTION('center_axis',(0.,0.,1.));
#9174=DIRECTION('ref_axis',(1.,0.,0.));
#9175=DIRECTION('center_axis',(0.,0.,1.));
#9176=DIRECTION('ref_axis',(1.,0.,0.));
#9177=DIRECTION('center_axis',(0.,0.,1.));
#9178=DIRECTION('ref_axis',(1.,0.,0.));
#9179=DIRECTION('',(0.,0.,-1.));
#9180=DIRECTION('center_axis',(0.,0.,1.));
#9181=DIRECTION('ref_axis',(1.,0.,0.));
#9182=DIRECTION('center_axis',(0.,0.,1.));
#9183=DIRECTION('ref_axis',(1.,0.,0.));
#9184=DIRECTION('center_axis',(0.,0.,1.));
#9185=DIRECTION('ref_axis',(1.,0.,0.));
#9186=DIRECTION('axis',(0.,0.,1.));
#9187=DIRECTION('refdir',(1.,0.,0.));
#9188=DIRECTION('center_axis',(0.,0.,-1.));
#9189=DIRECTION('ref_axis',(1.,0.,0.));
#9190=DIRECTION('',(0.,0.,-1.));
#9191=DIRECTION('center_axis',(0.,0.,-1.));
#9192=DIRECTION('ref_axis',(1.,0.,0.));
#9193=DIRECTION('center_axis',(0.,0.,-1.));
#9194=DIRECTION('ref_axis',(1.,0.,0.));
#9195=DIRECTION('',(0.,0.,-1.));
#9196=DIRECTION('center_axis',(0.,0.,-1.));
#9197=DIRECTION('ref_axis',(1.,0.,0.));
#9198=DIRECTION('center_axis',(0.,0.,-1.));
#9199=DIRECTION('ref_axis',(1.,0.,0.));
#9200=DIRECTION('',(0.,0.,-1.));
#9201=DIRECTION('center_axis',(0.,0.,-1.));
#9202=DIRECTION('ref_axis',(1.,0.,0.));
#9203=DIRECTION('',(0.,0.,-1.));
#9204=DIRECTION('center_axis',(0.,0.,-1.));
#9205=DIRECTION('ref_axis',(0.937385399639056,-0.348293859468591,0.));
#9206=DIRECTION('',(0.,0.,-1.));
#9207=DIRECTION('center_axis',(0.,0.,-1.));
#9208=DIRECTION('ref_axis',(1.,0.,0.));
#9209=DIRECTION('center_axis',(0.,0.,-1.));
#9210=DIRECTION('ref_axis',(0.28361887368566,0.958937085782627,0.));
#9211=DIRECTION('',(1.22464679914735E-16,8.07419868282478E-31,-1.));
#9212=DIRECTION('center_axis',(0.,0.,1.));
#9213=DIRECTION('ref_axis',(1.,6.71554824363804E-15,0.));
#9214=DIRECTION('center_axis',(0.,0.,-1.));
#9215=DIRECTION('ref_axis',(1.,6.71554824363804E-15,0.));
#9216=DIRECTION('',(1.22464679914735E-16,8.07419868282478E-31,-1.));
#9217=DIRECTION('center_axis',(0.,0.,-1.));
#9218=DIRECTION('ref_axis',(1.,6.71554824363804E-15,0.));
#9219=DIRECTION('',(1.22464679914735E-16,8.07419868282478E-31,-1.));
#9220=DIRECTION('center_axis',(0.,0.,-1.));
#9221=DIRECTION('ref_axis',(1.,6.71554824363804E-15,0.));
#9222=DIRECTION('',(1.22464679914735E-16,8.07419868282478E-31,-1.));
#9223=DIRECTION('center_axis',(0.,0.,-1.));
#9224=DIRECTION('ref_axis',(-0.60895050335979,-0.793208222636313,0.));
#9225=DIRECTION('',(1.22464679914735E-16,8.07419868282478E-31,-1.));
#9226=DIRECTION('center_axis',(0.,0.,-1.));
#9227=DIRECTION('ref_axis',(1.,6.71554824363804E-15,0.));
#9228=DIRECTION('center_axis',(0.,0.,-1.));
#9229=DIRECTION('ref_axis',(1.,6.71554824363804E-15,0.));
#9230=DIRECTION('center_axis',(0.,0.,1.));
#9231=DIRECTION('ref_axis',(1.,0.,0.));
#9232=DIRECTION('',(0.5,0.866025403784439,0.));
#9233=DIRECTION('',(-0.5,0.866025403784439,0.));
#9234=DIRECTION('',(-1.,0.,0.));
#9235=DIRECTION('',(-0.5,-0.866025403784439,0.));
#9236=DIRECTION('',(0.5,-0.866025403784439,0.));
#9237=DIRECTION('',(1.,-3.49629579342466E-16,0.));
#9238=DIRECTION('center_axis',(0.,0.,-1.));
#9239=DIRECTION('ref_axis',(1.,0.,0.));
#9240=DIRECTION('center_axis',(-3.49629579342466E-16,-1.,0.));
#9241=DIRECTION('ref_axis',(1.,-3.49629579342466E-16,0.));
#9242=DIRECTION('',(1.,-3.49629579342466E-16,0.));
#9243=DIRECTION('',(0.,0.,1.));
#9244=DIRECTION('',(0.,0.,1.));
#9245=DIRECTION('center_axis',(-0.866025403784439,-0.5,0.));
#9246=DIRECTION('ref_axis',(0.5,-0.866025403784439,0.));
#9247=DIRECTION('',(0.5,-0.866025403784439,0.));
#9248=DIRECTION('',(0.,0.,1.));
#9249=DIRECTION('center_axis',(-0.866025403784439,0.5,0.));
#9250=DIRECTION('ref_axis',(-0.5,-0.866025403784439,0.));
#9251=DIRECTION('',(-0.5,-0.866025403784439,0.));
#9252=DIRECTION('',(0.,0.,1.));
#9253=DIRECTION('center_axis',(0.,1.,0.));
#9254=DIRECTION('ref_axis',(-1.,0.,0.));
#9255=DIRECTION('',(-1.,0.,0.));
#9256=DIRECTION('',(0.,0.,1.));
#9257=DIRECTION('center_axis',(0.866025403784439,0.5,0.));
#9258=DIRECTION('ref_axis',(-0.5,0.866025403784439,0.));
#9259=DIRECTION('',(-0.5,0.866025403784439,0.));
#9260=DIRECTION('',(0.,0.,1.));
#9261=DIRECTION('center_axis',(0.866025403784439,-0.5,0.));
#9262=DIRECTION('ref_axis',(0.5,0.866025403784439,0.));
#9263=DIRECTION('',(0.5,0.866025403784439,0.));
#9264=DIRECTION('center_axis',(0.,0.,1.));
#9265=DIRECTION('ref_axis',(1.,0.,0.));
#9266=DIRECTION('',(0.,0.,1.));
#9267=DIRECTION('',(1.,0.,0.));
#9268=DIRECTION('',(0.,-1.22464679914735E-16,-1.));
#9269=DIRECTION('',(1.,0.,0.));
#9270=DIRECTION('',(0.,0.,1.));
#9271=DIRECTION('',(1.,0.,0.));
#9272=DIRECTION('',(0.,-1.22464679914735E-16,-1.));
#9273=DIRECTION('',(1.,0.,0.));
#9274=DIRECTION('',(0.,0.,1.));
#9275=DIRECTION('',(1.,0.,0.));
#9276=DIRECTION('',(0.,-1.22464679914735E-16,-1.));
#9277=DIRECTION('',(1.,0.,0.));
#9278=DIRECTION('',(0.,-1.22464679914735E-16,-1.));
#9279=DIRECTION('',(1.,0.,0.));
#9280=DIRECTION('',(0.,0.,1.));
#9281=DIRECTION('',(1.,0.,0.));
#9282=DIRECTION('axis',(0.,0.,1.));
#9283=DIRECTION('refdir',(1.,0.,0.));
#9284=DIRECTION('center_axis',(0.,0.,1.));
#9285=DIRECTION('ref_axis',(1.,0.,0.));
#9286=DIRECTION('center_axis',(0.,0.,-1.));
#9287=DIRECTION('ref_axis',(1.,0.,0.));
#9288=DIRECTION('',(0.,0.,-1.));
#9289=DIRECTION('center_axis',(0.,0.,-1.));
#9290=DIRECTION('ref_axis',(1.,0.,0.));
#9291=DIRECTION('center_axis',(0.,0.,1.));
#9292=DIRECTION('ref_axis',(1.,0.,0.));
#9293=DIRECTION('center_axis',(0.,0.,1.));
#9294=DIRECTION('ref_axis',(1.,0.,0.));
#9295=DIRECTION('',(0.,0.,-1.));
#9296=DIRECTION('center_axis',(0.,0.,1.));
#9297=DIRECTION('ref_axis',(1.,0.,0.));
#9298=DIRECTION('center_axis',(0.,0.,1.));
#9299=DIRECTION('ref_axis',(1.,0.,0.));
#9300=DIRECTION('center_axis',(0.,0.,1.));
#9301=DIRECTION('ref_axis',(1.,0.,0.));
#9302=DIRECTION('',(0.,0.,1.));
#9303=DIRECTION('',(1.,0.,0.));
#9304=DIRECTION('',(-6.12323398860133E-17,-1.22464679914735E-16,-1.));
#9305=DIRECTION('',(0.999999999999999,5.89805981832115E-17,-6.12323398860133E-17));
#9306=DIRECTION('',(0.,0.,1.));
#9307=DIRECTION('',(1.,0.,0.));
#9308=DIRECTION('',(0.,0.,1.));
#9309=DIRECTION('',(1.,0.,0.));
#9310=DIRECTION('',(0.,0.,1.));
#9311=DIRECTION('',(1.,0.,0.));
#9312=DIRECTION('',(0.,0.,1.));
#9313=DIRECTION('',(1.,0.,0.));
#9314=DIRECTION('',(-6.12323398860133E-17,-1.22464679914735E-16,-1.));
#9315=DIRECTION('',(0.999999999999999,-3.46944695195362E-18,-6.12323398860133E-17));
#9316=DIRECTION('',(0.,0.,1.));
#9317=DIRECTION('',(1.,0.,0.));
#9318=CARTESIAN_POINT('',(0.,0.,0.));
#9319=CARTESIAN_POINT('',(0.,0.,0.));
#9320=CARTESIAN_POINT('Origin',(6.,-2.5,0.3));
#9321=CARTESIAN_POINT('',(5.83,-2.5,0.6));
#9322=CARTESIAN_POINT('Origin',(6.,-2.5,0.6));
#9323=CARTESIAN_POINT('',(5.83,-2.5,0.));
#9324=CARTESIAN_POINT('',(5.83,-2.5,0.3));
#9325=CARTESIAN_POINT('Origin',(6.,-2.5,0.));
#9326=CARTESIAN_POINT('Origin',(15.2,-2.5,0.3));
#9327=CARTESIAN_POINT('',(15.03,-2.5,0.6));
#9328=CARTESIAN_POINT('Origin',(15.2,-2.5,0.6));
#9329=CARTESIAN_POINT('',(15.03,-2.5,0.));
#9330=CARTESIAN_POINT('',(15.03,-2.5,0.3));
#9331=CARTESIAN_POINT('Origin',(15.2,-2.5,0.));
#9332=CARTESIAN_POINT('Origin',(0.,0.,0.3));
#9333=CARTESIAN_POINT('',(-0.41,5.02105187650415E-17,0.6));
#9334=CARTESIAN_POINT('Origin',(0.,0.,0.6));
#9335=CARTESIAN_POINT('',(-0.41,5.02105187650415E-17,0.));
#9336=CARTESIAN_POINT('',(-0.41,5.02105187650415E-17,0.3));
#9337=CARTESIAN_POINT('Origin',(0.,0.,0.));
#9338=CARTESIAN_POINT('Origin',(-2.30284302574442,-0.0584079378788056,0.175));
#9339=CARTESIAN_POINT('',(-2.43506977313011,0.123638999134158,0.3));
#9340=CARTESIAN_POINT('',(-2.2,-0.2,0.3));
#9341=CARTESIAN_POINT('',(-2.72946351288801,0.528953957403482,0.3));
#9342=CARTESIAN_POINT('',(-2.2,-0.2,0.));
#9343=CARTESIAN_POINT('',(-2.2,-0.2,-4.89203798331893E-32));
#9344=CARTESIAN_POINT('',(-2.2,-0.2,0.));
#9345=CARTESIAN_POINT('Origin',(-4.25,2.62239583333333,0.15));
#9346=CARTESIAN_POINT('',(-6.3,-0.2,0.));
#9347=CARTESIAN_POINT('',(-6.06493022686989,0.123638999134159,0.3));
#9348=CARTESIAN_POINT('',(-6.3,-0.2,-4.89203798331893E-32));
#9349=CARTESIAN_POINT('Origin',(-4.25,2.62239583333333,0.));
#9350=CARTESIAN_POINT('Origin',(-4.25,2.62239583333333,0.3));
#9351=CARTESIAN_POINT('Origin',(-6.19715697425558,-0.0584079378788055,0.175));
#9352=CARTESIAN_POINT('',(-6.3,-0.2,0.3));
#9353=CARTESIAN_POINT('',(-5.70146423931269,0.624051140031634,0.3));
#9354=CARTESIAN_POINT('',(-6.3,-0.2,0.));
#9355=CARTESIAN_POINT('Origin',(-2.2,-0.2,0.));
#9356=CARTESIAN_POINT('',(-2.,0.0666666666666669,0.3));
#9357=CARTESIAN_POINT('',(-2.,0.0666666666666669,0.));
#9358=CARTESIAN_POINT('',(-2.,0.0666666666666667,0.));
#9359=CARTESIAN_POINT('',(-1.6,0.6,0.3));
#9360=CARTESIAN_POINT('',(-1.6,0.6,0.));
#9361=CARTESIAN_POINT('Origin',(-1.6,1.2,0.));
#9362=CARTESIAN_POINT('',(-2.4,1.8,0.));
#9363=CARTESIAN_POINT('',(-1.6,1.2,0.));
#9364=CARTESIAN_POINT('',(-2.4,1.8,0.));
#9365=CARTESIAN_POINT('',(-2.4,1.8,0.3));
#9366=CARTESIAN_POINT('',(-2.4,1.8,0.));
#9367=CARTESIAN_POINT('',(-1.6,1.2,0.3));
#9368=CARTESIAN_POINT('',(-2.4,1.8,0.3));
#9369=CARTESIAN_POINT('',(-1.6,1.2,0.));
#9370=CARTESIAN_POINT('Origin',(-6.3,1.38777878078145E-17,0.));
#9371=CARTESIAN_POINT('',(-6.3,0.2,0.));
#9372=CARTESIAN_POINT('Origin',(-6.3,1.38777878078145E-17,0.));
#9373=CARTESIAN_POINT('',(-6.3,0.2,0.3));
#9374=CARTESIAN_POINT('Origin',(-6.3,1.38777878078145E-17,0.3));
#9375=CARTESIAN_POINT('',(-6.3,0.2,0.));
#9376=CARTESIAN_POINT('Origin',(-1.81772727272727,-5.17241477272727,0.));
#9377=CARTESIAN_POINT('Origin',(-1.81772727272727,-5.17241477272727,0.));
#9378=CARTESIAN_POINT('Origin',(-1.81772727272727,-5.17241477272727,0.3));
#9379=CARTESIAN_POINT('Origin',(-4.05,0.467034919695243,0.3));
#9380=CARTESIAN_POINT('',(-2.,1.2,0.3));
#9381=CARTESIAN_POINT('',(-2.,0.833517459847621,0.3));
#9382=CARTESIAN_POINT('',(-2.625,1.2,0.3));
#9383=CARTESIAN_POINT('Origin',(-1.2,1.2,0.));
#9384=CARTESIAN_POINT('',(-2.,1.2,0.6));
#9385=CARTESIAN_POINT('',(-2.,1.2,0.));
#9386=CARTESIAN_POINT('',(-1.2,1.2,0.6));
#9387=CARTESIAN_POINT('',(-2.,1.2,0.6));
#9388=CARTESIAN_POINT('',(-1.2,1.2,0.));
#9389=CARTESIAN_POINT('',(-1.2,1.2,0.));
#9390=CARTESIAN_POINT('',(-2.,1.2,0.));
#9391=CARTESIAN_POINT('Origin',(-2.,1.2,0.));
#9392=CARTESIAN_POINT('',(-2.,0.,0.));
#9393=CARTESIAN_POINT('',(-2.,0.,0.));
#9394=CARTESIAN_POINT('',(-2.,0.,0.6));
#9395=CARTESIAN_POINT('',(-2.,0.,0.));
#9396=CARTESIAN_POINT('',(-2.,0.,0.6));
#9397=CARTESIAN_POINT('Origin',(-2.,0.,0.));
#9398=CARTESIAN_POINT('',(-1.4,0.,0.6));
#9399=CARTESIAN_POINT('',(-1.4,0.,0.));
#9400=CARTESIAN_POINT('',(-1.4,0.,0.));
#9401=CARTESIAN_POINT('',(-1.2,0.,0.6));
#9402=CARTESIAN_POINT('',(-1.2,0.,0.));
#9403=CARTESIAN_POINT('Origin',(-1.2,0.,0.));
#9404=CARTESIAN_POINT('',(-1.2,0.721110255092798,0.));
#9405=CARTESIAN_POINT('',(-1.2,0.721110255092798,0.6));
#9406=CARTESIAN_POINT('',(-1.2,0.721110255092798,0.));
#9407=CARTESIAN_POINT('',(-1.2,1.2,0.));
#9408=CARTESIAN_POINT('',(-1.2,1.2,0.6));
#9409=CARTESIAN_POINT('Origin',(0.,0.,0.));
#9410=CARTESIAN_POINT('',(0.518766934059614,-1.30033875129767,0.));
#9411=CARTESIAN_POINT('Origin',(0.,0.,0.));
#9412=CARTESIAN_POINT('',(0.518766934059614,-1.30033875129767,0.6));
#9413=CARTESIAN_POINT('',(0.518766934059614,-1.30033875129767,0.));
#9414=CARTESIAN_POINT('Origin',(0.,0.,0.6));
#9415=CARTESIAN_POINT('Origin',(0.,0.,0.));
#9416=CARTESIAN_POINT('',(0.993295878967653,0.986591757935306,0.6));
#9417=CARTESIAN_POINT('Origin',(0.,0.,0.6));
#9418=CARTESIAN_POINT('',(0.993295878967653,0.986591757935306,0.));
#9419=CARTESIAN_POINT('',(0.993295878967653,0.986591757935306,0.));
#9420=CARTESIAN_POINT('Origin',(0.,0.,0.));
#9421=CARTESIAN_POINT('Origin',(0.,0.,0.6));
#9422=CARTESIAN_POINT('',(0.544110909138566,-1.31501157897496,0.6));
#9423=CARTESIAN_POINT('',(0.,-1.,0.6));
#9424=CARTESIAN_POINT('',(3.46875216140085,-3.00822493554786,0.6));
#9425=CARTESIAN_POINT('Origin',(2.1,-2.,0.6));
#9426=CARTESIAN_POINT('',(3.8,-3.2,0.6));
#9427=CARTESIAN_POINT('',(0.,-1.,0.6));
#9428=CARTESIAN_POINT('',(16.4,-3.2,0.6));
#9429=CARTESIAN_POINT('',(3.8,-3.2,0.6));
#9430=CARTESIAN_POINT('',(16.4,-1.8,0.6));
#9431=CARTESIAN_POINT('',(16.4,-3.2,0.6));
#9432=CARTESIAN_POINT('',(3.8,-1.8,0.6));
#9433=CARTESIAN_POINT('',(16.4,-1.8,0.6));
#9434=CARTESIAN_POINT('',(3.78654599313281,-1.78654599313281,0.6));
#9435=CARTESIAN_POINT('',(3.8,-1.8,0.6));
#9436=CARTESIAN_POINT('',(2.31345400686719,-0.313454006867188,0.6));
#9437=CARTESIAN_POINT('Origin',(2.1,-2.,0.6));
#9438=CARTESIAN_POINT('',(1.,1.,0.6));
#9439=CARTESIAN_POINT('',(3.8,-1.8,0.6));
#9440=CARTESIAN_POINT('',(1.,1.,0.6));
#9441=CARTESIAN_POINT('',(3.3,-2.,0.6));
#9442=CARTESIAN_POINT('Origin',(2.1,-2.,0.6));
#9443=CARTESIAN_POINT('Origin',(2.1,-2.,0.1));
#9444=CARTESIAN_POINT('',(0.9,-2.,0.));
#9445=CARTESIAN_POINT('Origin',(2.1,-2.,0.));
#9446=CARTESIAN_POINT('',(1.,-2.,0.1));
#9447=CARTESIAN_POINT('Origin',(0.9,-2.,0.1));
#9448=CARTESIAN_POINT('Origin',(2.1,-2.,0.1));
#9449=CARTESIAN_POINT('Origin',(2.1,-2.,0.3));
#9450=CARTESIAN_POINT('',(3.2,-2.,0.5));
#9451=CARTESIAN_POINT('',(1.,-2.,0.5));
#9452=CARTESIAN_POINT('Origin',(2.1,-2.,0.5));
#9453=CARTESIAN_POINT('Origin',(2.1,-2.,0.5));
#9454=CARTESIAN_POINT('',(1.,-2.,0.3));
#9455=CARTESIAN_POINT('Origin',(0.,0.,0.));
#9456=CARTESIAN_POINT('',(1.,1.,0.));
#9457=CARTESIAN_POINT('',(1.,1.,0.));
#9458=CARTESIAN_POINT('',(2.31345400686719,-0.313454006867188,0.));
#9459=CARTESIAN_POINT('',(3.8,-1.8,0.));
#9460=CARTESIAN_POINT('',(3.78654599313281,-1.78654599313281,0.));
#9461=CARTESIAN_POINT('Origin',(2.1,-2.,0.));
#9462=CARTESIAN_POINT('',(3.8,-1.8,0.));
#9463=CARTESIAN_POINT('',(3.8,-1.8,0.));
#9464=CARTESIAN_POINT('',(16.4,-1.8,0.));
#9465=CARTESIAN_POINT('',(16.4,-1.8,0.));
#9466=CARTESIAN_POINT('',(16.4,-3.2,0.));
#9467=CARTESIAN_POINT('',(16.4,-3.2,0.));
#9468=CARTESIAN_POINT('',(3.8,-3.2,0.));
#9469=CARTESIAN_POINT('',(3.8,-3.2,0.));
#9470=CARTESIAN_POINT('',(3.46875216140085,-3.00822493554786,0.));
#9471=CARTESIAN_POINT('',(0.,-1.,0.));
#9472=CARTESIAN_POINT('',(0.544110909138566,-1.31501157897496,0.));
#9473=CARTESIAN_POINT('Origin',(2.1,-2.,0.));
#9474=CARTESIAN_POINT('',(0.,-1.,0.));
#9475=CARTESIAN_POINT('Origin',(2.1,-2.,0.5));
#9476=CARTESIAN_POINT('Origin',(3.3,-2.,0.5));
#9477=CARTESIAN_POINT('Origin',(2.1,-2.,0.));
#9478=CARTESIAN_POINT('',(2.31345400686719,-0.313454006867188,0.));
#9479=CARTESIAN_POINT('',(3.78654599313281,-1.78654599313281,0.));
#9480=CARTESIAN_POINT('Origin',(2.1,-2.,0.));
#9481=CARTESIAN_POINT('',(0.544110909138566,-1.31501157897496,0.));
#9482=CARTESIAN_POINT('',(3.46875216140085,-3.00822493554786,0.));
#9483=CARTESIAN_POINT('Origin',(0.,-1.,0.));
#9484=CARTESIAN_POINT('',(3.8,-3.2,0.));
#9485=CARTESIAN_POINT('Origin',(3.8,-1.8,0.));
#9486=CARTESIAN_POINT('',(3.8,-1.8,0.));
#9487=CARTESIAN_POINT('Origin',(0.,-1.,0.));
#9488=CARTESIAN_POINT('Origin',(1.,1.,0.));
#9489=CARTESIAN_POINT('',(1.,1.,0.));
#9490=CARTESIAN_POINT('Origin',(3.8,-1.8,0.));
#9491=CARTESIAN_POINT('Origin',(16.4,-1.8,0.));
#9492=CARTESIAN_POINT('',(16.4,-1.8,0.));
#9493=CARTESIAN_POINT('Origin',(16.4,-3.2,0.));
#9494=CARTESIAN_POINT('',(16.4,-3.2,0.));
#9495=CARTESIAN_POINT('Origin',(3.8,-3.2,0.));
#9496=CARTESIAN_POINT('',(0.,0.,0.));
#9497=CARTESIAN_POINT('Origin',(6.,-2.5,0.3));
#9498=CARTESIAN_POINT('',(5.83,-2.5,0.6));
#9499=CARTESIAN_POINT('Origin',(6.,-2.5,0.6));
#9500=CARTESIAN_POINT('',(5.83,-2.5,0.));
#9501=CARTESIAN_POINT('',(5.83,-2.5,0.3));
#9502=CARTESIAN_POINT('Origin',(6.,-2.5,0.));
#9503=CARTESIAN_POINT('Origin',(15.2,-2.5,0.3));
#9504=CARTESIAN_POINT('',(15.03,-2.5,0.6));
#9505=CARTESIAN_POINT('Origin',(15.2,-2.5,0.6));
#9506=CARTESIAN_POINT('',(15.03,-2.5,0.));
#9507=CARTESIAN_POINT('',(15.03,-2.5,0.3));
#9508=CARTESIAN_POINT('Origin',(15.2,-2.5,0.));
#9509=CARTESIAN_POINT('Origin',(0.,0.,0.3));
#9510=CARTESIAN_POINT('',(-0.41,5.02105187650415E-17,0.6));
#9511=CARTESIAN_POINT('Origin',(0.,0.,0.6));
#9512=CARTESIAN_POINT('',(-0.41,5.02105187650415E-17,0.));
#9513=CARTESIAN_POINT('',(-0.41,5.02105187650415E-17,0.3));
#9514=CARTESIAN_POINT('Origin',(0.,0.,0.));
#9515=CARTESIAN_POINT('Origin',(-2.2,-0.3,0.));
#9516=CARTESIAN_POINT('',(-2.,0.,0.));
#9517=CARTESIAN_POINT('',(-2.,0.,0.4));
#9518=CARTESIAN_POINT('',(-2.,0.,0.));
#9519=CARTESIAN_POINT('',(-2.2,-0.3,0.4));
#9520=CARTESIAN_POINT('',(-1.6,0.6,0.4));
#9521=CARTESIAN_POINT('',(-2.2,-0.3,0.));
#9522=CARTESIAN_POINT('',(-2.2,-0.3,0.));
#9523=CARTESIAN_POINT('',(-1.6,0.6,0.));
#9524=CARTESIAN_POINT('Origin',(-1.6,1.2,0.));
#9525=CARTESIAN_POINT('',(-2.4,1.8,0.));
#9526=CARTESIAN_POINT('',(-1.6,1.2,0.));
#9527=CARTESIAN_POINT('',(-2.4,1.8,0.));
#9528=CARTESIAN_POINT('',(-2.4,1.8,0.4));
#9529=CARTESIAN_POINT('',(-2.4,1.8,0.));
#9530=CARTESIAN_POINT('',(-1.6,1.2,0.4));
#9531=CARTESIAN_POINT('',(-2.4,1.8,0.4));
#9532=CARTESIAN_POINT('',(-1.6,1.2,0.));
#9533=CARTESIAN_POINT('Origin',(-4.2,1.928125,0.));
#9534=CARTESIAN_POINT('',(-6.2,-0.3,0.));
#9535=CARTESIAN_POINT('Origin',(-4.2,1.928125,0.));
#9536=CARTESIAN_POINT('',(-6.2,-0.3,0.4));
#9537=CARTESIAN_POINT('Origin',(-4.2,1.928125,0.4));
#9538=CARTESIAN_POINT('',(-6.2,-0.3,0.));
#9539=CARTESIAN_POINT('Origin',(-6.2,2.77555756156289E-17,0.));
#9540=CARTESIAN_POINT('',(-6.2,0.300000000000001,0.));
#9541=CARTESIAN_POINT('Origin',(-6.2,2.77555756156289E-17,0.));
#9542=CARTESIAN_POINT('',(-6.2,0.3,0.4));
#9543=CARTESIAN_POINT('Origin',(-6.2,2.77555756156289E-17,0.4));
#9544=CARTESIAN_POINT('',(-6.2,0.300000000000001,0.));
#9545=CARTESIAN_POINT('Origin',(-1.79797381546135,-5.28846633416459,0.));
#9546=CARTESIAN_POINT('Origin',(-1.79797381546135,-5.28846633416459,0.));
#9547=CARTESIAN_POINT('Origin',(-1.79797381546135,-5.28846633416459,0.4));
#9548=CARTESIAN_POINT('Origin',(-4.05,0.367020331620548,0.4));
#9549=CARTESIAN_POINT('',(-2.,1.2,0.4));
#9550=CARTESIAN_POINT('',(-2.625,1.2,0.4));
#9551=CARTESIAN_POINT('',(-2.,0.783510165810274,0.4));
#9552=CARTESIAN_POINT('Origin',(-1.2,1.2,0.));
#9553=CARTESIAN_POINT('',(-2.,1.2,0.6));
#9554=CARTESIAN_POINT('',(-2.,1.2,0.));
#9555=CARTESIAN_POINT('',(-1.2,1.2,0.6));
#9556=CARTESIAN_POINT('',(-2.,1.2,0.6));
#9557=CARTESIAN_POINT('',(-1.2,1.2,0.));
#9558=CARTESIAN_POINT('',(-1.2,1.2,0.));
#9559=CARTESIAN_POINT('',(-2.,1.2,0.));
#9560=CARTESIAN_POINT('Origin',(-2.,1.2,0.));
#9561=CARTESIAN_POINT('',(-2.,0.,0.6));
#9562=CARTESIAN_POINT('',(-2.,0.,0.));
#9563=CARTESIAN_POINT('',(-2.,0.,0.6));
#9564=CARTESIAN_POINT('Origin',(-2.,0.,0.));
#9565=CARTESIAN_POINT('',(-1.4,0.,0.6));
#9566=CARTESIAN_POINT('',(-1.4,0.,0.));
#9567=CARTESIAN_POINT('',(-1.4,0.,0.));
#9568=CARTESIAN_POINT('',(-1.2,0.,0.6));
#9569=CARTESIAN_POINT('',(-1.2,0.,0.));
#9570=CARTESIAN_POINT('Origin',(-1.2,0.,0.));
#9571=CARTESIAN_POINT('',(-1.2,0.721110255092798,0.));
#9572=CARTESIAN_POINT('',(-1.2,0.721110255092798,0.6));
#9573=CARTESIAN_POINT('',(-1.2,0.721110255092798,0.));
#9574=CARTESIAN_POINT('',(-1.2,1.2,0.));
#9575=CARTESIAN_POINT('',(-1.2,1.2,0.6));
#9576=CARTESIAN_POINT('Origin',(0.,0.,0.));
#9577=CARTESIAN_POINT('',(0.518766934059614,-1.30033875129767,0.));
#9578=CARTESIAN_POINT('Origin',(0.,0.,0.));
#9579=CARTESIAN_POINT('',(0.518766934059614,-1.30033875129767,0.6));
#9580=CARTESIAN_POINT('',(0.518766934059614,-1.30033875129767,0.));
#9581=CARTESIAN_POINT('Origin',(0.,0.,0.6));
#9582=CARTESIAN_POINT('Origin',(0.,0.,0.));
#9583=CARTESIAN_POINT('',(0.993295878967653,0.986591757935306,0.6));
#9584=CARTESIAN_POINT('Origin',(0.,0.,0.6));
#9585=CARTESIAN_POINT('',(0.993295878967653,0.986591757935306,0.));
#9586=CARTESIAN_POINT('',(0.993295878967653,0.986591757935306,0.));
#9587=CARTESIAN_POINT('Origin',(0.,0.,0.));
#9588=CARTESIAN_POINT('Origin',(0.,0.,0.6));
#9589=CARTESIAN_POINT('',(0.544110909138566,-1.31501157897496,0.6));
#9590=CARTESIAN_POINT('',(0.,-1.,0.6));
#9591=CARTESIAN_POINT('',(3.46875216140085,-3.00822493554786,0.6));
#9592=CARTESIAN_POINT('Origin',(2.1,-2.,0.6));
#9593=CARTESIAN_POINT('',(3.8,-3.2,0.6));
#9594=CARTESIAN_POINT('',(0.,-1.,0.6));
#9595=CARTESIAN_POINT('',(16.4,-3.2,0.6));
#9596=CARTESIAN_POINT('',(3.8,-3.2,0.6));
#9597=CARTESIAN_POINT('',(16.4,-1.8,0.6));
#9598=CARTESIAN_POINT('',(16.4,-3.2,0.6));
#9599=CARTESIAN_POINT('',(3.8,-1.8,0.6));
#9600=CARTESIAN_POINT('',(16.4,-1.8,0.6));
#9601=CARTESIAN_POINT('',(3.78654599313281,-1.78654599313281,0.6));
#9602=CARTESIAN_POINT('',(3.8,-1.8,0.6));
#9603=CARTESIAN_POINT('',(2.31345400686719,-0.313454006867188,0.6));
#9604=CARTESIAN_POINT('Origin',(2.1,-2.,0.6));
#9605=CARTESIAN_POINT('',(1.,1.,0.6));
#9606=CARTESIAN_POINT('',(3.8,-1.8,0.6));
#9607=CARTESIAN_POINT('',(1.,1.,0.6));
#9608=CARTESIAN_POINT('',(3.3,-2.,0.6));
#9609=CARTESIAN_POINT('Origin',(2.1,-2.,0.6));
#9610=CARTESIAN_POINT('Origin',(2.1,-2.,0.1));
#9611=CARTESIAN_POINT('',(0.9,-2.,0.));
#9612=CARTESIAN_POINT('Origin',(2.1,-2.,0.));
#9613=CARTESIAN_POINT('',(1.,-2.,0.1));
#9614=CARTESIAN_POINT('Origin',(0.9,-2.,0.1));
#9615=CARTESIAN_POINT('Origin',(2.1,-2.,0.1));
#9616=CARTESIAN_POINT('Origin',(2.1,-2.,0.3));
#9617=CARTESIAN_POINT('',(3.2,-2.,0.5));
#9618=CARTESIAN_POINT('',(1.,-2.,0.5));
#9619=CARTESIAN_POINT('Origin',(2.1,-2.,0.5));
#9620=CARTESIAN_POINT('Origin',(2.1,-2.,0.5));
#9621=CARTESIAN_POINT('',(1.,-2.,0.3));
#9622=CARTESIAN_POINT('Origin',(0.,0.,0.));
#9623=CARTESIAN_POINT('',(1.,1.,0.));
#9624=CARTESIAN_POINT('',(1.,1.,0.));
#9625=CARTESIAN_POINT('',(2.31345400686719,-0.313454006867188,0.));
#9626=CARTESIAN_POINT('',(3.8,-1.8,0.));
#9627=CARTESIAN_POINT('',(3.78654599313281,-1.78654599313281,0.));
#9628=CARTESIAN_POINT('Origin',(2.1,-2.,0.));
#9629=CARTESIAN_POINT('',(3.8,-1.8,0.));
#9630=CARTESIAN_POINT('',(3.8,-1.8,0.));
#9631=CARTESIAN_POINT('',(16.4,-1.8,0.));
#9632=CARTESIAN_POINT('',(16.4,-1.8,0.));
#9633=CARTESIAN_POINT('',(16.4,-3.2,0.));
#9634=CARTESIAN_POINT('',(16.4,-3.2,0.));
#9635=CARTESIAN_POINT('',(3.8,-3.2,0.));
#9636=CARTESIAN_POINT('',(3.8,-3.2,0.));
#9637=CARTESIAN_POINT('',(3.46875216140085,-3.00822493554786,0.));
#9638=CARTESIAN_POINT('',(0.,-1.,0.));
#9639=CARTESIAN_POINT('',(0.544110909138566,-1.31501157897496,0.));
#9640=CARTESIAN_POINT('Origin',(2.1,-2.,0.));
#9641=CARTESIAN_POINT('',(0.,-1.,0.));
#9642=CARTESIAN_POINT('Origin',(2.1,-2.,0.5));
#9643=CARTESIAN_POINT('Origin',(3.3,-2.,0.5));
#9644=CARTESIAN_POINT('Origin',(2.1,-2.,0.));
#9645=CARTESIAN_POINT('',(2.31345400686719,-0.313454006867188,0.));
#9646=CARTESIAN_POINT('',(3.78654599313281,-1.78654599313281,0.));
#9647=CARTESIAN_POINT('Origin',(2.1,-2.,0.));
#9648=CARTESIAN_POINT('',(0.544110909138566,-1.31501157897496,0.));
#9649=CARTESIAN_POINT('',(3.46875216140085,-3.00822493554786,0.));
#9650=CARTESIAN_POINT('Origin',(0.,-1.,0.));
#9651=CARTESIAN_POINT('',(3.8,-3.2,0.));
#9652=CARTESIAN_POINT('Origin',(3.8,-1.8,0.));
#9653=CARTESIAN_POINT('',(3.8,-1.8,0.));
#9654=CARTESIAN_POINT('Origin',(0.,-1.,0.));
#9655=CARTESIAN_POINT('Origin',(1.,1.,0.));
#9656=CARTESIAN_POINT('',(1.,1.,0.));
#9657=CARTESIAN_POINT('Origin',(3.8,-1.8,0.));
#9658=CARTESIAN_POINT('Origin',(16.4,-1.8,0.));
#9659=CARTESIAN_POINT('',(16.4,-1.8,0.));
#9660=CARTESIAN_POINT('Origin',(16.4,-3.2,0.));
#9661=CARTESIAN_POINT('',(16.4,-3.2,0.));
#9662=CARTESIAN_POINT('Origin',(3.8,-3.2,0.));
#9663=CARTESIAN_POINT('',(0.,0.,0.));
#9664=CARTESIAN_POINT('Origin',(0.,0.,0.75));
#9665=CARTESIAN_POINT('',(-0.3,-3.67394039744206E-17,0.7));
#9666=CARTESIAN_POINT('Origin',(0.,0.,0.7));
#9667=CARTESIAN_POINT('',(-0.3,-3.67394039744206E-17,0.8));
#9668=CARTESIAN_POINT('',(-0.3,-3.67394039744206E-17,0.75));
#9669=CARTESIAN_POINT('Origin',(0.,0.,0.8));
#9670=CARTESIAN_POINT('Origin',(0.7,0.,0.7));
#9671=CARTESIAN_POINT('',(-0.4,4.89858719658941E-17,0.7));
#9672=CARTESIAN_POINT('Origin',(0.,0.,0.7));
#9673=CARTESIAN_POINT('Origin',(0.3,0.,0.8));
#9674=CARTESIAN_POINT('',(-0.4,-4.89858719658941E-17,0.8));
#9675=CARTESIAN_POINT('Origin',(0.,0.,0.8));
#9676=CARTESIAN_POINT('Origin',(0.,0.,-0.7));
#9677=CARTESIAN_POINT('',(-0.4,-4.89858719658941E-17,0.9));
#9678=CARTESIAN_POINT('Origin',(0.,0.,0.9));
#9679=CARTESIAN_POINT('',(-0.4,-4.89858719658941E-17,-0.7));
#9680=CARTESIAN_POINT('Origin',(0.,0.,-0.7));
#9681=CARTESIAN_POINT('',(-0.6,-7.34788079488412E-17,-0.7));
#9682=CARTESIAN_POINT('Origin',(0.,0.,-0.7));
#9683=CARTESIAN_POINT('',(-0.4,-4.89858719658941E-17,-0.7));
#9684=CARTESIAN_POINT('Origin',(0.,0.,-0.7));
#9685=CARTESIAN_POINT('Origin',(0.,0.,-0.8));
#9686=CARTESIAN_POINT('',(-0.6,-7.34788079488412E-17,-0.8));
#9687=CARTESIAN_POINT('',(-0.6,-7.34788079488412E-17,-0.8));
#9688=CARTESIAN_POINT('Origin',(0.,0.,-0.8));
#9689=CARTESIAN_POINT('Origin',(0.,0.,-0.8));
#9690=CARTESIAN_POINT('Origin',(0.,0.,-0.7));
#9691=CARTESIAN_POINT('',(-0.4,-4.89858719658941E-17,-0.7));
#9692=CARTESIAN_POINT('Origin',(0.,0.,0.9));
#9693=CARTESIAN_POINT('',(0.,0.,0.));
#9694=CARTESIAN_POINT('Origin',(-0.1,0.,0.1));
#9695=CARTESIAN_POINT('',(-0.1,0.282842712474619,0.));
#9696=CARTESIAN_POINT('',(-0.1,0.282842712474619,0.1));
#9697=CARTESIAN_POINT('',(-0.1,0.282842712474619,0.));
#9698=CARTESIAN_POINT('',(-0.1,0.591607978309962,0.));
#9699=CARTESIAN_POINT('',(-0.1,0.,0.));
#9700=CARTESIAN_POINT('',(-0.1,0.591607978309962,0.1));
#9701=CARTESIAN_POINT('',(-0.1,0.591607978309962,0.));
#9702=CARTESIAN_POINT('',(-0.1,0.,0.1));
#9703=CARTESIAN_POINT('Origin',(0.1,1.2,0.1));
#9704=CARTESIAN_POINT('',(0.1,0.282842712474619,0.1));
#9705=CARTESIAN_POINT('',(0.1,0.282842712474619,0.));
#9706=CARTESIAN_POINT('',(0.1,0.282842712474619,0.));
#9707=CARTESIAN_POINT('',(0.1,0.591607978309962,0.1));
#9708=CARTESIAN_POINT('',(0.1,0.6,0.1));
#9709=CARTESIAN_POINT('',(0.1,0.591607978309962,0.));
#9710=CARTESIAN_POINT('',(0.1,0.591607978309962,0.));
#9711=CARTESIAN_POINT('',(0.1,0.6,0.));
#9712=CARTESIAN_POINT('Origin',(0.,0.,0.));
#9713=CARTESIAN_POINT('Origin',(0.,0.,0.));
#9714=CARTESIAN_POINT('Origin',(0.,0.,0.));
#9715=CARTESIAN_POINT('Origin',(0.,0.,0.));
#9716=CARTESIAN_POINT('Origin',(0.,0.,0.1));
#9717=CARTESIAN_POINT('Origin',(0.,0.,0.));
#9718=CARTESIAN_POINT('Origin',(0.,0.,0.1));
#9719=CARTESIAN_POINT('Origin',(0.,0.,0.1));
#9720=CARTESIAN_POINT('',(0.,0.,0.));
#9721=CARTESIAN_POINT('',(0.,0.,0.));
#9722=CARTESIAN_POINT('Origin',(6.87409734069396,-2.22251806091942E-16,
0.7));
#9723=CARTESIAN_POINT('',(3.31825992066485,1.2493322588334,0.7));
#9724=CARTESIAN_POINT('',(4.3,1.27917501057225,0.7));
#9725=CARTESIAN_POINT('Ctrl Pts',(3.31826243508713,1.24933270901874,0.7));
#9726=CARTESIAN_POINT('Ctrl Pts',(3.64552542112514,1.25866821321074,0.7));
#9727=CARTESIAN_POINT('Ctrl Pts',(3.97277304530853,1.26856018917077,0.7));
#9728=CARTESIAN_POINT('Ctrl Pts',(4.30000000005992,1.27917501058303,0.7));
#9729=CARTESIAN_POINT('',(4.3,-1.27917501057184,0.7));
#9730=CARTESIAN_POINT('',(4.3,0.742407407407408,0.7));
#9731=CARTESIAN_POINT('',(3.31825992075695,-1.24933225883136,0.7));
#9732=CARTESIAN_POINT('Ctrl Pts',(4.3000000000599,-1.27917501058303,0.7));
#9733=CARTESIAN_POINT('Ctrl Pts',(3.97277304533917,-1.26856018917177,0.7));
#9734=CARTESIAN_POINT('Ctrl Pts',(3.64552542118644,-1.25866821321259,0.7));
#9735=CARTESIAN_POINT('Ctrl Pts',(3.3182624351791,-1.24933270902137,0.7));
#9736=CARTESIAN_POINT('',(3.26759951430388,-1.24789152572578,0.7));
#9737=CARTESIAN_POINT('Ctrl Pts',(3.26760216044043,-1.24789199949781,0.7));
#9738=CARTESIAN_POINT('Ctrl Pts',(3.27154046708102,-1.24840675231115,0.699999999449966));
#9739=CARTESIAN_POINT('Ctrl Pts',(3.27549053112987,-1.2488275353013,0.699997549264952));
#9740=CARTESIAN_POINT('Ctrl Pts',(3.27944900419773,-1.24915404112413,0.699995443099811));
#9741=CARTESIAN_POINT('Ctrl Pts',(3.28202272903949,-1.24936632907779,0.699994073710794));
#9742=CARTESIAN_POINT('Ctrl Pts',(3.28459959180148,-1.24953872742098,0.699992815093061));
#9743=CARTESIAN_POINT('Ctrl Pts',(3.28717866899733,-1.24967118132558,0.699992046536556));
#9744=CARTESIAN_POINT('Ctrl Pts',(3.28888409507617,-1.24975876704947,0.699991538325205));
#9745=CARTESIAN_POINT('Ctrl Pts',(3.29059037034979,-1.2498288805585,0.699991238158591));
#9746=CARTESIAN_POINT('Ctrl Pts',(3.29229723346923,-1.24988151179005,0.69999118215758));
#9747=CARTESIAN_POINT('Ctrl Pts',(3.29393274317941,-1.24993194283473,0.699991128497625));
#9748=CARTESIAN_POINT('Ctrl Pts',(3.29556870469678,-1.24996631998408,0.699991298652463));
#9749=CARTESIAN_POINT('Ctrl Pts',(3.29720488848534,-1.24998463806557,0.699991673963628));
#9750=CARTESIAN_POINT('Ctrl Pts',(3.29943508678369,-1.25000960650399,0.699992185531049));
#9751=CARTESIAN_POINT('Ctrl Pts',(3.30166551218918,-1.25000473681137,0.699993084765318));
#9752=CARTESIAN_POINT('Ctrl Pts',(3.30389557412726,-1.24997002667259,0.699994176731177));
#9753=CARTESIAN_POINT('Ctrl Pts',(3.30868977915254,-1.24989540653807,0.699996524248132));
#9754=CARTESIAN_POINT('Ctrl Pts',(3.31348068594496,-1.24968290539118,0.699999999312134));
#9755=CARTESIAN_POINT('Ctrl Pts',(3.3182624351791,-1.24933270902137,0.7));
#9756=CARTESIAN_POINT('',(1.1,-1.19266190204492,0.7));
#9757=CARTESIAN_POINT('Ctrl Pts',(3.26760216044045,-1.24789199949781,0.7));
#9758=CARTESIAN_POINT('Ctrl Pts',(2.54512260523322,-1.2274084473838,0.7));
#9759=CARTESIAN_POINT('Ctrl Pts',(1.82256951666701,-1.20959509718369,0.7));
#9760=CARTESIAN_POINT('Ctrl Pts',(1.09999999999999,-1.19266190204553,0.7));
#9761=CARTESIAN_POINT('',(1.1,1.19266190204492,0.7));
#9762=CARTESIAN_POINT('',(1.1,-0.696450594095222,0.7));
#9763=CARTESIAN_POINT('',(3.26759952419083,1.24789152650872,0.7));
#9764=CARTESIAN_POINT('Ctrl Pts',(1.09999999999999,1.19266190204553,0.7));
#9765=CARTESIAN_POINT('Ctrl Pts',(1.82256951996781,1.20959509726105,0.7));
#9766=CARTESIAN_POINT('Ctrl Pts',(2.54512261183467,1.22740844754655,0.7));
#9767=CARTESIAN_POINT('Ctrl Pts',(3.26760217034162,1.24789199977852,0.7));
#9768=CARTESIAN_POINT('Ctrl Pts',(3.3182624351791,1.24933270902137,0.7));
#9769=CARTESIAN_POINT('Ctrl Pts',(3.3143012451848,1.2496228108833,0.699999999430174));
#9770=CARTESIAN_POINT('Ctrl Pts',(3.31033365565543,1.24981842655856,0.699997549220164));
#9771=CARTESIAN_POINT('Ctrl Pts',(3.30636302717881,1.24991943948955,0.699995443052606));
#9772=CARTESIAN_POINT('Ctrl Pts',(3.30378139908369,1.24998511620097,0.699994073661998));
#9773=CARTESIAN_POINT('Ctrl Pts',(3.3011989045204,1.25001078941611,0.699992815050698));
#9774=CARTESIAN_POINT('Ctrl Pts',(3.29861646861803,1.2499964568765,0.699992046505716));
#9775=CARTESIAN_POINT('Ctrl Pts',(3.2969088217217,1.24998697942277,0.699991538302026));
#9776=CARTESIAN_POINT('Ctrl Pts',(3.29520131971864,1.24996000972381,0.699991238145114));
#9777=CARTESIAN_POINT('Ctrl Pts',(3.29349422410899,1.24991555258537,0.699991182154076));
#9778=CARTESIAN_POINT('Ctrl Pts',(3.29185849176351,1.24987295392896,0.699991128503682));
#9779=CARTESIAN_POINT('Ctrl Pts',(3.29022322047391,1.2498143016413,0.699991298668259));
#9780=CARTESIAN_POINT('Ctrl Pts',(3.28858863969825,1.2497396036024,0.699991673987721));
#9781=CARTESIAN_POINT('Ctrl Pts',(3.286360626573,1.24963778654105,0.699992185566407));
#9782=CARTESIAN_POINT('Ctrl Pts',(3.28413408201674,1.24950616665997,0.699993084809042));
#9783=CARTESIAN_POINT('Ctrl Pts',(3.2819095957713,1.24934477520901,0.699994176777649));
#9784=CARTESIAN_POINT('Ctrl Pts',(3.27712738077041,1.24899781481787,0.699996524298861));
#9785=CARTESIAN_POINT('Ctrl Pts',(3.27235629258357,1.24851338385513,0.699999999330822));
#9786=CARTESIAN_POINT('Ctrl Pts',(3.26760217026193,1.24789200078152,0.699999999999999));
#9787=CARTESIAN_POINT('',(3.15,1.,0.7));
#9788=CARTESIAN_POINT('Origin',(3.3,1.,0.7));
#9789=CARTESIAN_POINT('',(3.15,-1.,0.7));
#9790=CARTESIAN_POINT('Origin',(3.3,-1.,0.7));
#9791=CARTESIAN_POINT('',(1.6,-4.89858719658941E-17,0.7));
#9792=CARTESIAN_POINT('Origin',(2.,0.,0.7));
#9793=CARTESIAN_POINT('Origin',(9.9,-1.,0.8));
#9794=CARTESIAN_POINT('',(9.75,-1.,0.9));
#9795=CARTESIAN_POINT('Origin',(9.9,-1.,0.9));
#9796=CARTESIAN_POINT('',(9.75,-1.,0.7));
#9797=CARTESIAN_POINT('',(9.75,-1.,0.8));
#9798=CARTESIAN_POINT('Origin',(9.9,-1.,0.7));
#9799=CARTESIAN_POINT('Origin',(3.3,-1.,0.8));
#9800=CARTESIAN_POINT('',(3.15,-1.,0.9));
#9801=CARTESIAN_POINT('Origin',(3.3,-1.,0.9));
#9802=CARTESIAN_POINT('',(3.15,-1.,0.8));
#9803=CARTESIAN_POINT('Origin',(3.3,1.,0.8));
#9804=CARTESIAN_POINT('',(3.15,1.,0.9));
#9805=CARTESIAN_POINT('Origin',(3.3,1.,0.9));
#9806=CARTESIAN_POINT('',(3.15,1.,0.8));
#9807=CARTESIAN_POINT('Origin',(9.9,1.,0.8));
#9808=CARTESIAN_POINT('',(9.75,1.,0.9));
#9809=CARTESIAN_POINT('Origin',(9.9,1.,0.9));
#9810=CARTESIAN_POINT('',(9.75,1.,0.7));
#9811=CARTESIAN_POINT('',(9.75,1.,0.8));
#9812=CARTESIAN_POINT('Origin',(9.9,1.,0.7));
#9813=CARTESIAN_POINT('Origin',(2.,0.,0.75));
#9814=CARTESIAN_POINT('',(1.7,3.67394039744206E-17,0.9));
#9815=CARTESIAN_POINT('Origin',(2.,0.,0.9));
#9816=CARTESIAN_POINT('',(1.7,3.67394039744206E-17,0.6));
#9817=CARTESIAN_POINT('',(1.7,3.67394039744206E-17,0.75));
#9818=CARTESIAN_POINT('Origin',(2.,0.,0.6));
#9819=CARTESIAN_POINT('Origin',(2.,0.,0.6));
#9820=CARTESIAN_POINT('',(1.83,-2.0818995585505E-17,0.6));
#9821=CARTESIAN_POINT('Origin',(2.,0.,0.6));
#9822=CARTESIAN_POINT('Origin',(11.2,0.,0.75));
#9823=CARTESIAN_POINT('',(10.9,3.67394039744206E-17,0.9));
#9824=CARTESIAN_POINT('Origin',(11.2,0.,0.9));
#9825=CARTESIAN_POINT('',(10.9,3.67394039744206E-17,0.6));
#9826=CARTESIAN_POINT('',(10.9,3.67394039744206E-17,0.75));
#9827=CARTESIAN_POINT('Origin',(11.2,0.,0.6));
#9828=CARTESIAN_POINT('Origin',(11.2,0.,0.6));
#9829=CARTESIAN_POINT('',(11.03,-2.0818995585505E-17,0.6));
#9830=CARTESIAN_POINT('Origin',(11.2,0.,0.6));
#9831=CARTESIAN_POINT('Origin',(2.,0.,0.45));
#9832=CARTESIAN_POINT('',(1.83,-2.0818995585505E-17,0.32));
#9833=CARTESIAN_POINT('',(1.83,2.0818995585505E-17,0.45));
#9834=CARTESIAN_POINT('Origin',(2.,0.,0.32));
#9835=CARTESIAN_POINT('Origin',(11.2,0.,0.45));
#9836=CARTESIAN_POINT('',(11.03,-2.0818995585505E-17,0.32));
#9837=CARTESIAN_POINT('',(11.03,2.0818995585505E-17,0.45));
#9838=CARTESIAN_POINT('Origin',(11.2,0.,0.32));
#9839=CARTESIAN_POINT('Origin',(12.4,-0.72,0.32));
#9840=CARTESIAN_POINT('',(0.200274469199584,-0.72,0.));
#9841=CARTESIAN_POINT('',(0.217044958570157,-0.72,0.32));
#9842=CARTESIAN_POINT('',(0.225070308370679,-0.72,0.473132796510599));
#9843=CARTESIAN_POINT('',(0.,-0.72,0.));
#9844=CARTESIAN_POINT('',(9.63649764092939,-0.72,0.));
#9845=CARTESIAN_POINT('',(0.0167704893705732,-0.72,0.32));
#9846=CARTESIAN_POINT('',(0.0253444014197637,-0.72,0.483599987759188));
#9847=CARTESIAN_POINT('',(-0.1,-0.72,0.32));
#9848=CARTESIAN_POINT('Origin',(12.4,-0.72,0.32));
#9849=CARTESIAN_POINT('',(0.9,-0.72,0.32));
#9850=CARTESIAN_POINT('',(0.9,-0.72,0.));
#9851=CARTESIAN_POINT('',(0.9,-0.72,0.16));
#9852=CARTESIAN_POINT('',(1.1,-0.72,0.32));
#9853=CARTESIAN_POINT('',(-0.1,-0.72,0.32));
#9854=CARTESIAN_POINT('',(1.1,-0.72,0.));
#9855=CARTESIAN_POINT('',(1.1,-0.72,0.16));
#9856=CARTESIAN_POINT('',(9.63649764092939,-0.72,0.));
#9857=CARTESIAN_POINT('Origin',(12.4,-0.72,0.32));
#9858=CARTESIAN_POINT('',(4.3,-0.72,0.32));
#9859=CARTESIAN_POINT('',(4.3,-0.72,0.));
#9860=CARTESIAN_POINT('',(4.3,-0.72,0.16));
#9861=CARTESIAN_POINT('',(4.5,-0.72,0.32));
#9862=CARTESIAN_POINT('',(-0.1,-0.72,0.32));
#9863=CARTESIAN_POINT('',(4.5,-0.72,0.));
#9864=CARTESIAN_POINT('',(4.5,-0.72,0.16));
#9865=CARTESIAN_POINT('',(9.63649764092939,-0.72,0.));
#9866=CARTESIAN_POINT('Origin',(12.4,-0.72,0.32));
#9867=CARTESIAN_POINT('',(8.7,-0.72,0.32));
#9868=CARTESIAN_POINT('',(8.7,-0.72,0.));
#9869=CARTESIAN_POINT('',(8.7,-0.72,0.16));
#9870=CARTESIAN_POINT('',(8.9,-0.72,0.32));
#9871=CARTESIAN_POINT('',(-0.1,-0.72,0.32));
#9872=CARTESIAN_POINT('',(8.9,-0.72,0.));
#9873=CARTESIAN_POINT('',(8.9,-0.72,0.16));
#9874=CARTESIAN_POINT('',(9.63649764092939,-0.72,0.));
#9875=CARTESIAN_POINT('Origin',(-0.0999999999999996,0.72,0.32));
#9876=CARTESIAN_POINT('',(0.217044958570158,0.72,0.32));
#9877=CARTESIAN_POINT('',(0.200274469199584,0.72,0.));
#9878=CARTESIAN_POINT('',(0.207951231396534,0.72,0.146481348799182));
#9879=CARTESIAN_POINT('',(0.0167704893705736,0.72,0.32));
#9880=CARTESIAN_POINT('',(12.4,0.72,0.32));
#9881=CARTESIAN_POINT('',(0.,0.72,0.));
#9882=CARTESIAN_POINT('',(0.00822532444561912,0.72,0.156948540047771));
#9883=CARTESIAN_POINT('',(3.38649764092939,0.72,0.));
#9884=CARTESIAN_POINT('Origin',(-0.0999999999999996,0.72,0.32));
#9885=CARTESIAN_POINT('',(0.9,0.72,0.));
#9886=CARTESIAN_POINT('',(0.9,0.72,0.32));
#9887=CARTESIAN_POINT('',(0.9,0.72,0.16));
#9888=CARTESIAN_POINT('',(1.1,0.72,0.));
#9889=CARTESIAN_POINT('',(3.38649764092939,0.72,0.));
#9890=CARTESIAN_POINT('',(1.1,0.72,0.32));
#9891=CARTESIAN_POINT('',(1.1,0.72,0.16));
#9892=CARTESIAN_POINT('',(12.4,0.72,0.32));
#9893=CARTESIAN_POINT('Origin',(-0.0999999999999996,0.72,0.32));
#9894=CARTESIAN_POINT('',(4.3,0.72,0.));
#9895=CARTESIAN_POINT('',(4.3,0.72,0.32));
#9896=CARTESIAN_POINT('',(4.3,0.72,0.16));
#9897=CARTESIAN_POINT('',(4.5,0.72,0.));
#9898=CARTESIAN_POINT('',(3.38649764092939,0.72,0.));
#9899=CARTESIAN_POINT('',(4.5,0.72,0.32));
#9900=CARTESIAN_POINT('',(4.5,0.72,0.16));
#9901=CARTESIAN_POINT('',(12.4,0.72,0.32));
#9902=CARTESIAN_POINT('Origin',(6.15,0.,0.32));
#9903=CARTESIAN_POINT('',(1.6,-4.89858719658941E-17,0.32));
#9904=CARTESIAN_POINT('Origin',(2.,0.,0.32));
#9905=CARTESIAN_POINT('Origin',(6.15,0.,0.32));
#9906=CARTESIAN_POINT('',(10.8,-4.89858719658942E-17,0.32));
#9907=CARTESIAN_POINT('Origin',(11.2,0.,0.32));
#9908=CARTESIAN_POINT('Origin',(6.15,0.,0.32));
#9909=CARTESIAN_POINT('',(0.217044958570157,-0.75,0.32));
#9910=CARTESIAN_POINT('',(0.0167704893705736,-0.75,0.32));
#9911=CARTESIAN_POINT('Origin',(6.15,0.,0.32));
#9912=CARTESIAN_POINT('',(0.9,0.696450594095222,0.32));
#9913=CARTESIAN_POINT('',(1.1,-0.696450594095222,0.32));
#9914=CARTESIAN_POINT('Origin',(6.15,0.,0.32));
#9915=CARTESIAN_POINT('',(4.3,0.742407407407408,0.32));
#9916=CARTESIAN_POINT('',(4.5,-0.742407407407408,0.32));
#9917=CARTESIAN_POINT('Origin',(6.15,0.,0.32));
#9918=CARTESIAN_POINT('',(8.7,0.72,0.32));
#9919=CARTESIAN_POINT('',(8.7,0.844259259259259,0.32));
#9920=CARTESIAN_POINT('',(8.9,0.72,0.32));
#9921=CARTESIAN_POINT('',(12.4,0.72,0.32));
#9922=CARTESIAN_POINT('',(8.9,-0.844259259259259,0.32));
#9923=CARTESIAN_POINT('Origin',(-0.0999999999999996,0.72,0.32));
#9924=CARTESIAN_POINT('',(8.7,0.72,0.));
#9925=CARTESIAN_POINT('',(8.7,0.72,0.16));
#9926=CARTESIAN_POINT('',(8.9,0.72,0.));
#9927=CARTESIAN_POINT('',(3.38649764092939,0.72,0.));
#9928=CARTESIAN_POINT('',(8.9,0.72,0.16));
#9929=CARTESIAN_POINT('Origin',(12.4,1.99376954809806,0.));
#9930=CARTESIAN_POINT('',(12.4,1.91212902562343,0.));
#9931=CARTESIAN_POINT('',(12.4,-1.91212902562343,0.));
#9932=CARTESIAN_POINT('',(12.4,1.99376954809806,0.));
#9933=CARTESIAN_POINT('',(12.4,-1.8833055216247,0.604732563714112));
#9934=CARTESIAN_POINT('Ctrl Pts',(12.4,-1.8833055216247,0.604732563714112));
#9935=CARTESIAN_POINT('Ctrl Pts',(12.4,-1.88809880980762,0.504101072758768));
#9936=CARTESIAN_POINT('Ctrl Pts',(12.4,-1.89289370245628,0.403468941627095));
#9937=CARTESIAN_POINT('Ctrl Pts',(12.4,-1.90250151416087,0.201891903194028));
#9938=CARTESIAN_POINT('Ctrl Pts',(12.4,-1.90731451170285,0.100945553925438));
#9939=CARTESIAN_POINT('Ctrl Pts',(12.4,-1.91212902562343,0.));
#9940=CARTESIAN_POINT('',(12.4,-1.78288409287054,0.7));
#9941=CARTESIAN_POINT('Ctrl Pts',(12.4000000030461,-1.78288409409899,0.7));
#9942=CARTESIAN_POINT('Ctrl Pts',(12.4000000066823,-1.79082830277209,0.699999997040196));
#9943=CARTESIAN_POINT('Ctrl Pts',(12.4000021328137,-1.79871128857748,0.699006690321208));
#9944=CARTESIAN_POINT('Ctrl Pts',(12.4000039827682,-1.8063921320806,0.697119229445379));
#9945=CARTESIAN_POINT('Ctrl Pts',(12.4000049365067,-1.81035196808589,0.69614615460905));
#9946=CARTESIAN_POINT('Ctrl Pts',(12.4000058167808,-1.81425808325963,0.694934510320783));
#9947=CARTESIAN_POINT('Ctrl Pts',(12.400006432968,-1.81808986884151,0.693492707237305));
#9948=CARTESIAN_POINT('Ctrl Pts',(12.4000076352846,-1.82556652433459,0.690679432664999));
#9949=CARTESIAN_POINT('Ctrl Pts',(12.4000076271954,-1.83268048852469,0.687023315130674));
#9950=CARTESIAN_POINT('Ctrl Pts',(12.4000063864816,-1.83928589538344,0.682605693351404));
#9951=CARTESIAN_POINT('Ctrl Pts',(12.4000055969106,-1.84348947395919,0.679794387301037));
#9952=CARTESIAN_POINT('Ctrl Pts',(12.400004329084,-1.84748689691167,0.676673627174617));
#9953=CARTESIAN_POINT('Ctrl Pts',(12.4000032503406,-1.8512341074341,0.673255429390325));
#9954=CARTESIAN_POINT('Ctrl Pts',(12.4000023796213,-1.85425870830395,0.670496394655072));
#9955=CARTESIAN_POINT('Ctrl Pts',(12.4000016297172,-1.85710218072175,0.667559826261508));
#9956=CARTESIAN_POINT('Ctrl Pts',(12.4000016274617,-1.859744520612,0.664455546516084));
#9957=CARTESIAN_POINT('Ctrl Pts',(12.4000016230979,-1.86485672743849,0.658449612092435));
#9958=CARTESIAN_POINT('Ctrl Pts',(12.4000041080363,-1.86921906069885,0.651817317967817));
#9959=CARTESIAN_POINT('Ctrl Pts',(12.40000495371,-1.8727702927896,0.64472299566344));
#9960=CARTESIAN_POINT('Ctrl Pts',(12.4000050555652,-1.8731980125259,0.643868536819953));
#9961=CARTESIAN_POINT('Ctrl Pts',(12.4000051394069,-1.87361391018412,0.643007349425002));
#9962=CARTESIAN_POINT('Ctrl Pts',(12.4000052029357,-1.87401783114888,0.642139703315781));
#9963=CARTESIAN_POINT('Ctrl Pts',(12.4000057294153,-1.87736522853405,0.634949295858174));
#9964=CARTESIAN_POINT('Ctrl Pts',(12.4000043880804,-1.87985460663586,0.627401584261416));
#9965=CARTESIAN_POINT('Ctrl Pts',(12.4000025112034,-1.88143175301701,0.619663949188762));
#9966=CARTESIAN_POINT('Ctrl Pts',(12.4000013193515,-1.88243327046239,0.614750406220363));
#9967=CARTESIAN_POINT('Ctrl Pts',(12.4,-1.88306607129604,0.609759643802656));
#9968=CARTESIAN_POINT('Ctrl Pts',(12.4,-1.8833055216247,0.604732563714112));
#9969=CARTESIAN_POINT('',(12.4,1.78288409287164,0.7));
#9970=CARTESIAN_POINT('',(12.4,0.99688477404903,0.7));
#9971=CARTESIAN_POINT('',(12.4,1.8833055216247,0.604732563714112));
#9972=CARTESIAN_POINT('Ctrl Pts',(12.4,1.8833055216247,0.604732563714112));
#9973=CARTESIAN_POINT('Ctrl Pts',(12.4,1.88292893537322,0.612638709665068));
#9974=CARTESIAN_POINT('Ctrl Pts',(12.4000029905988,1.88158186833012,0.620459457162159));
#9975=CARTESIAN_POINT('Ctrl Pts',(12.400004351969,1.87934739482834,0.62803467841275));
#9976=CARTESIAN_POINT('Ctrl Pts',(12.4000050124983,1.87826324073514,0.631710133556493));
#9977=CARTESIAN_POINT('Ctrl Pts',(12.4000053733669,1.87696936339782,0.63532777623417));
#9978=CARTESIAN_POINT('Ctrl Pts',(12.4000053391329,1.87547104796815,0.638868146717817));
#9979=CARTESIAN_POINT('Ctrl Pts',(12.4000052683671,1.872373843052,0.646186534188034));
#9980=CARTESIAN_POINT('Ctrl Pts',(12.4000032465668,1.86844110215533,0.653093304890266));
#9981=CARTESIAN_POINT('Ctrl Pts',(12.4000021327941,1.86374151467895,0.659427433016556));
#9982=CARTESIAN_POINT('Ctrl Pts',(12.4000018304335,1.86246569800928,0.66114698527342));
#9983=CARTESIAN_POINT('Ctrl Pts',(12.4000016226794,1.86113309763036,0.662824214875179));
#9984=CARTESIAN_POINT('Ctrl Pts',(12.400001625255,1.85974452038344,0.664455546516227));
#9985=CARTESIAN_POINT('Ctrl Pts',(12.4000016287814,1.85784336180007,0.666689070188443));
#9986=CARTESIAN_POINT('Ctrl Pts',(12.400002024929,1.85583728779192,0.668836587948716));
#9987=CARTESIAN_POINT('Ctrl Pts',(12.4000025639666,1.85373364862045,0.670894373083513));
#9988=CARTESIAN_POINT('Ctrl Pts',(12.400004021536,1.84804536272624,0.676458668669153));
#9989=CARTESIAN_POINT('Ctrl Pts',(12.4000062945443,1.84171268252251,0.681305055194542));
#9990=CARTESIAN_POINT('Ctrl Pts',(12.4000070319583,1.83490078417639,0.685381489016216));
#9991=CARTESIAN_POINT('Ctrl Pts',(12.4000075068619,1.8305138392177,0.688006761722114));
#9992=CARTESIAN_POINT('Ctrl Pts',(12.4000074483741,1.82592714021755,0.69031203082117));
#9993=CARTESIAN_POINT('Ctrl Pts',(12.4000068708525,1.82117863971551,0.692273867243687));
#9994=CARTESIAN_POINT('Ctrl Pts',(12.4000059767178,1.81382688138917,0.695311236040001));
#9995=CARTESIAN_POINT('Ctrl Pts',(12.4000038254996,1.80617119073902,0.697493343451155));
#9996=CARTESIAN_POINT('Ctrl Pts',(12.4000020685374,1.7983596509798,0.698751345219246));
#9997=CARTESIAN_POINT('Ctrl Pts',(12.4000009204513,1.79325520389048,0.699573385900268));
#9998=CARTESIAN_POINT('Ctrl Pts',(12.400000005426,1.78808359082883,0.699999998062804));
#9999=CARTESIAN_POINT('Ctrl Pts',(12.4000000030461,1.78288409409899,0.7));
#10000=CARTESIAN_POINT('Ctrl Pts',(12.4,1.91212902562343,0.));
#10001=CARTESIAN_POINT('Ctrl Pts',(12.4,1.90731404243129,0.1009553931071));
#10002=CARTESIAN_POINT('Ctrl Pts',(12.4,1.9025005759122,0.201911581737034));
#10003=CARTESIAN_POINT('Ctrl Pts',(12.4,1.89289276481806,0.403488620176902));
#10004=CARTESIAN_POINT('Ctrl Pts',(12.4,1.88809834114759,0.504110911924693));
#10005=CARTESIAN_POINT('Ctrl Pts',(12.4,1.8833055216247,0.604732563714112));
#10006=CARTESIAN_POINT('Origin',(8.9,-1.68851851851852,0.));
#10007=CARTESIAN_POINT('',(8.9,1.62420669932031,0.));
#10008=CARTESIAN_POINT('',(8.9,-1.68851851851852,0.));
#10009=CARTESIAN_POINT('',(8.9,1.59320117118329,0.605106081470792));
#10010=CARTESIAN_POINT('Ctrl Pts',(8.9,1.59320117118329,0.605106081470792));
#10011=CARTESIAN_POINT('Ctrl Pts',(8.9,1.59837103562161,0.504197738990529));
#10012=CARTESIAN_POINT('Ctrl Pts',(8.9,1.60354126123154,0.403288838380538));
#10013=CARTESIAN_POINT('Ctrl Pts',(8.9,1.61387642009944,0.201587196710533));
#10014=CARTESIAN_POINT('Ctrl Pts',(8.9,1.61904141157348,0.100793304842659));
#10015=CARTESIAN_POINT('Ctrl Pts',(8.9,1.62420669932031,0.));
#10016=CARTESIAN_POINT('',(8.9,1.49312521822106,0.7));
#10017=CARTESIAN_POINT('Ctrl Pts',(8.9,1.49312521822106,0.7));
#10018=CARTESIAN_POINT('Ctrl Pts',(8.9,1.50104136823484,0.7));
#10019=CARTESIAN_POINT('Ctrl Pts',(8.90000131173634,1.50889623314995,0.699007530025307));
#10020=CARTESIAN_POINT('Ctrl Pts',(8.90000245364087,1.51654949575132,0.697121675771258));
#10021=CARTESIAN_POINT('Ctrl Pts',(8.9000030153269,1.52031402289636,0.696194051841344));
#10022=CARTESIAN_POINT('Ctrl Pts',(8.90000353645954,1.52402976767023,0.695049421358208));
#10023=CARTESIAN_POINT('Ctrl Pts',(8.90000391188735,1.52767894577544,0.693695149285802));
#10024=CARTESIAN_POINT('Ctrl Pts',(8.90000468147812,1.53515940869299,0.690919022244083));
#10025=CARTESIAN_POINT('Ctrl Pts',(8.90000470661952,1.54227958804117,0.687295426711095));
#10026=CARTESIAN_POINT('Ctrl Pts',(8.9000039635008,1.54889410374269,0.682907715777054));
#10027=CARTESIAN_POINT('Ctrl Pts',(8.90000349228854,1.55308837416723,0.680125464281631));
#10028=CARTESIAN_POINT('Ctrl Pts',(8.90000272405863,1.55707914411963,0.677034908766328));
#10029=CARTESIAN_POINT('Ctrl Pts',(8.90000205379677,1.56082314136721,0.673648333128258));
#10030=CARTESIAN_POINT('Ctrl Pts',(8.90000149471997,1.56394607304962,0.670823532879853));
#10031=CARTESIAN_POINT('Ctrl Pts',(8.90000100172653,1.56687805273397,0.667809941545923));
#10032=CARTESIAN_POINT('Ctrl Pts',(8.90000100003,1.56959740049228,0.664618488856983));
#10033=CARTESIAN_POINT('Ctrl Pts',(8.90000099684156,1.57470809805256,0.658620525035968));
#10034=CARTESIAN_POINT('Ctrl Pts',(8.90000253934467,1.57907071782202,0.651995745956818));
#10035=CARTESIAN_POINT('Ctrl Pts',(8.90000305932469,1.58262507990443,0.644909256877938));
#10036=CARTESIAN_POINT('Ctrl Pts',(8.90000311559331,1.58300970826793,0.644142406277414));
#10037=CARTESIAN_POINT('Ctrl Pts',(8.9000031627798,1.58338482682255,0.643370127200485));
#10038=CARTESIAN_POINT('Ctrl Pts',(8.90000319981124,1.58375032531468,0.642592615892991));
#10039=CARTESIAN_POINT('Ctrl Pts',(8.90000354178946,1.58712563340961,0.635412448897651));
#10040=CARTESIAN_POINT('Ctrl Pts',(8.90000272882427,1.58964525157545,0.627871187463612));
#10041=CARTESIAN_POINT('Ctrl Pts',(8.90000156924769,1.59125549206429,0.620136848214628));
#10042=CARTESIAN_POINT('Ctrl Pts',(8.90000082792478,1.59228492658837,0.615192247765769));
#10043=CARTESIAN_POINT('Ctrl Pts',(8.89999999997262,1.59294182914154,0.610168076493048));
#10044=CARTESIAN_POINT('Ctrl Pts',(8.9000000009702,1.5932011715731,0.605106081469384));
#10045=CARTESIAN_POINT('',(8.9,-1.49312521822001,0.7));
#10046=CARTESIAN_POINT('',(8.9,-0.844259259259259,0.7));
#10047=CARTESIAN_POINT('',(8.9,-1.59320117118329,0.605106081470792));
#10048=CARTESIAN_POINT('Ctrl Pts',(8.90000000097019,-1.5932011715731,0.605106081469384));
#10049=CARTESIAN_POINT('Ctrl Pts',(8.89999999941083,-1.59279578158415,0.613018716877257));
#10050=CARTESIAN_POINT('Ctrl Pts',(8.90000185372291,-1.59142151714118,0.620841302874248));
#10051=CARTESIAN_POINT('Ctrl Pts',(8.90000269095591,-1.58916270068609,0.628413601005994));
#10052=CARTESIAN_POINT('Ctrl Pts',(8.90000316003867,-1.58789713677684,0.632656188846207));
#10053=CARTESIAN_POINT('Ctrl Pts',(8.90000337414869,-1.58635289833986,0.636820251299613));
#10054=CARTESIAN_POINT('Ctrl Pts',(8.90000326408749,-1.58453800492682,0.640875626603871));
#10055=CARTESIAN_POINT('Ctrl Pts',(8.9000030675631,-1.58129734600662,0.648116871770122));
#10056=CARTESIAN_POINT('Ctrl Pts',(8.90000169351568,-1.5772322800227,0.654932667693845));
#10057=CARTESIAN_POINT('Ctrl Pts',(8.90000116172667,-1.57240747726376,0.66116027211862));
#10058=CARTESIAN_POINT('Ctrl Pts',(8.90000106146602,-1.57149783490479,0.662334391157823));
#10059=CARTESIAN_POINT('Ctrl Pts',(8.90000099955281,-1.57056105641498,0.663487533005214));
#10060=CARTESIAN_POINT('Ctrl Pts',(8.90000100072893,-1.56959740053727,0.664618488856962));
#10061=CARTESIAN_POINT('Ctrl Pts',(8.9000010030487,-1.56769671285427,0.666849154291726));
#10062=CARTESIAN_POINT('Ctrl Pts',(8.90000124864079,-1.56569149899762,0.668993559652069));
#10063=CARTESIAN_POINT('Ctrl Pts',(8.90000158179872,-1.56358911460694,0.671047966011734));
#10064=CARTESIAN_POINT('Ctrl Pts',(8.90000248280001,-1.55790336961918,0.676603957919834));
#10065=CARTESIAN_POINT('Ctrl Pts',(8.90000387848177,-1.55157399841983,0.681441805123218));
#10066=CARTESIAN_POINT('Ctrl Pts',(8.90000432886686,-1.54476515293017,0.68550782533293));
#10067=CARTESIAN_POINT('Ctrl Pts',(8.9000046162921,-1.54041990676133,0.688102664467623));
#10068=CARTESIAN_POINT('Ctrl Pts',(8.90000458123012,-1.53587841548674,0.69038248607508));
#10069=CARTESIAN_POINT('Ctrl Pts',(8.90000422571091,-1.53117752164703,0.692323975790708));
#10070=CARTESIAN_POINT('Ctrl Pts',(8.90000367147839,-1.52384911813356,0.695350638493274));
#10071=CARTESIAN_POINT('Ctrl Pts',(8.9000023358238,-1.51621796414731,0.697522741667433));
#10072=CARTESIAN_POINT('Ctrl Pts',(8.90000125519218,-1.50843132129101,0.698770821080692));
#10073=CARTESIAN_POINT('Ctrl Pts',(8.90000055451733,-1.5033825102871,0.699580068042664));
#10074=CARTESIAN_POINT('Ctrl Pts',(8.9,-1.49826772866746,0.7));
#10075=CARTESIAN_POINT('Ctrl Pts',(8.9,-1.49312521822106,0.7));
#10076=CARTESIAN_POINT('',(8.9,-1.62420669932031,0.));
#10077=CARTESIAN_POINT('Ctrl Pts',(8.9,-1.62420669932031,0.));
#10078=CARTESIAN_POINT('Ctrl Pts',(8.9,-1.61904139377919,0.100793652073202));
#10079=CARTESIAN_POINT('Ctrl Pts',(8.9,-1.61387638451174,0.201587891198165));
#10080=CARTESIAN_POINT('Ctrl Pts',(8.9,-1.60354122564866,0.403289532862703));
#10081=CARTESIAN_POINT('Ctrl Pts',(8.9,-1.59837101783099,0.50419808623799));
#10082=CARTESIAN_POINT('Ctrl Pts',(8.9,-1.59320117118329,0.605106081470792));
#10083=CARTESIAN_POINT('',(8.9,-1.68851851851852,0.));
#10084=CARTESIAN_POINT('Origin',(4.5,-1.48481481481482,0.));
#10085=CARTESIAN_POINT('',(4.5,1.41772989878425,0.));
#10086=CARTESIAN_POINT('',(4.5,-1.48481481481482,0.));
#10087=CARTESIAN_POINT('',(4.5,1.38566996325095,0.605286533624017));
#10088=CARTESIAN_POINT('Ctrl Pts',(4.5,1.38566996325095,0.605286533624017));
#10089=CARTESIAN_POINT('Ctrl Pts',(4.5,1.3910232158183,0.504222354021684));
#10090=CARTESIAN_POINT('Ctrl Pts',(4.5,1.39637635187357,0.403158168247774));
#10091=CARTESIAN_POINT('Ctrl Pts',(4.5,1.4070629957395,0.201395990303158));
#10092=CARTESIAN_POINT('Ctrl Pts',(4.5,1.41239650438775,0.100697998177668));
#10093=CARTESIAN_POINT('Ctrl Pts',(4.5,1.41772989878425,0.));
#10094=CARTESIAN_POINT('',(4.5,1.28575421950843,0.7));
#10095=CARTESIAN_POINT('Ctrl Pts',(4.5,1.28575421950843,0.7));
#10096=CARTESIAN_POINT('Ctrl Pts',(4.5,1.29366545802379,0.7));
#10097=CARTESIAN_POINT('Ctrl Pts',(4.50000067540813,1.30151306508378,0.699006020085879));
#10098=CARTESIAN_POINT('Ctrl Pts',(4.50000126278178,1.30915682219698,0.697118891599074));
#10099=CARTESIAN_POINT('Ctrl Pts',(4.50000159346398,1.31346013814185,0.696056467716811));
#10100=CARTESIAN_POINT('Ctrl Pts',(4.50000189442328,1.31769890045703,0.694709922559592));
#10101=CARTESIAN_POINT('Ctrl Pts',(4.50000208642664,1.32184639782974,0.693090275295953));
#10102=CARTESIAN_POINT('Ctrl Pts',(4.50000243009859,1.32927011415192,0.690191225399894));
#10103=CARTESIAN_POINT('Ctrl Pts',(4.50000235826664,1.33632110693134,0.686451804482762));
#10104=CARTESIAN_POINT('Ctrl Pts',(4.50000192249634,1.34285330390028,0.681953677325188));
#10105=CARTESIAN_POINT('Ctrl Pts',(4.5000016824508,1.3464515866709,0.679475868782656));
#10106=CARTESIAN_POINT('Ctrl Pts',(4.50000134086274,1.34989218134371,0.676766953538005));
#10107=CARTESIAN_POINT('Ctrl Pts',(4.50000103767597,1.35314674504257,0.67383503027087));
#10108=CARTESIAN_POINT('Ctrl Pts',(4.50000074242034,1.35631617169348,0.670979804009792));
#10109=CARTESIAN_POINT('Ctrl Pts',(4.50000047986374,1.35928994516467,0.667930335702103));
#10110=CARTESIAN_POINT('Ctrl Pts',(4.5000004798165,1.36204555935344,0.66469809744354));
#10111=CARTESIAN_POINT('Ctrl Pts',(4.5000004797289,1.36715559606013,0.658704204607119));
#10112=CARTESIAN_POINT('Ctrl Pts',(4.50000128456446,1.3715183542993,0.652083197653858));
#10113=CARTESIAN_POINT('Ctrl Pts',(4.50000155892095,1.37507421485048,0.645000595057188));
#10114=CARTESIAN_POINT('Ctrl Pts',(4.50000158702893,1.37543851484667,0.644274978272754));
#10115=CARTESIAN_POINT('Ctrl Pts',(4.50000161091379,1.37579430519483,0.643544496675346));
#10116=CARTESIAN_POINT('Ctrl Pts',(4.50000163009343,1.37614149316233,0.642809317076966));
#10117=CARTESIAN_POINT('Ctrl Pts',(4.50000181728783,1.37953006709248,0.635633923185928));
#10118=CARTESIAN_POINT('Ctrl Pts',(4.50000140772507,1.38206400387968,0.628095594687559));
#10119=CARTESIAN_POINT('Ctrl Pts',(4.50000081194859,1.38368993781387,0.620362729373495));
#10120=CARTESIAN_POINT('Ctrl Pts',(4.50000042990035,1.38473258588096,0.615403944208116));
#10121=CARTESIAN_POINT('Ctrl Pts',(4.49999999988018,1.38540098970406,0.610364492806037));
#10122=CARTESIAN_POINT('Ctrl Pts',(4.50000000014037,1.38566996330298,0.605286533623957));
#10123=CARTESIAN_POINT('',(4.5,-1.28575421950842,0.7));
#10124=CARTESIAN_POINT('',(4.5,-0.742407407407408,0.7));
#10125=CARTESIAN_POINT('',(4.5,-1.38566996325095,0.605286533624017));
#10126=CARTESIAN_POINT('Ctrl Pts',(4.50000000014037,-1.38566996330298,0.605286533623957));
#10127=CARTESIAN_POINT('Ctrl Pts',(4.49999999973491,-1.38525081272033,0.613199687771457));
#10128=CARTESIAN_POINT('Ctrl Pts',(4.50000095642016,-1.38386419754969,0.62102180968747));
#10129=CARTESIAN_POINT('Ctrl Pts',(4.50000138305812,-1.38159414679432,0.628592503408469));
#10130=CARTESIAN_POINT('Ctrl Pts',(4.50000162118259,-1.38032713666619,0.632818023740444));
#10131=CARTESIAN_POINT('Ctrl Pts',(4.50000172745986,-1.37878391728058,0.636965253716347));
#10132=CARTESIAN_POINT('Ctrl Pts',(4.50000166716583,-1.37697237493585,0.641004309729874));
#10133=CARTESIAN_POINT('Ctrl Pts',(4.50000155916287,-1.37372741146613,0.648239354085419));
#10134=CARTESIAN_POINT('Ctrl Pts',(4.50000084040372,-1.36965973349804,0.655049237033139));
#10135=CARTESIAN_POINT('Ctrl Pts',(4.50000056390271,-1.36483316768901,0.661270759279915));
#10136=CARTESIAN_POINT('Ctrl Pts',(4.50000051219424,-1.36393055121024,0.662434246679675));
#10137=CARTESIAN_POINT('Ctrl Pts',(4.50000048023544,-1.3630012658104,0.663577087492372));
#10138=CARTESIAN_POINT('Ctrl Pts',(4.50000048056391,-1.36204555937839,0.664698097443534));
#10139=CARTESIAN_POINT('Ctrl Pts',(4.50000048121673,-1.36014610273268,0.666926093123284));
#10140=CARTESIAN_POINT('Ctrl Pts',(4.50000060829837,-1.35814231322364,0.669067903674665));
#10141=CARTESIAN_POINT('Ctrl Pts',(4.50000078085101,-1.35604151212276,0.671119765431539));
#10142=CARTESIAN_POINT('Ctrl Pts',(4.50000124774248,-1.3503571825734,0.676671675324794));
#10143=CARTESIAN_POINT('Ctrl Pts',(4.50000197143062,-1.34402953514766,0.681505303070731));
#10144=CARTESIAN_POINT('Ctrl Pts',(4.50000220836427,-1.33722229030693,0.685566265232058));
#10145=CARTESIAN_POINT('Ctrl Pts',(4.50000235894787,-1.33289593407788,0.688147216755564));
#10146=CARTESIAN_POINT('Ctrl Pts',(4.50000234488938,-1.32837489877041,0.690415387400166));
#10147=CARTESIAN_POINT('Ctrl Pts',(4.50000216490635,-1.32369554581057,0.69234752884452));
#10148=CARTESIAN_POINT('Ctrl Pts',(4.50000188343739,-1.31637767466938,0.695369135087455));
#10149=CARTESIAN_POINT('Ctrl Pts',(4.50000119588393,-1.3087575932273,0.697536490026807));
#10150=CARTESIAN_POINT('Ctrl Pts',(4.50000064127173,-1.30098224657147,0.698779892333419));
#10151=CARTESIAN_POINT('Ctrl Pts',(4.50000028296845,-1.29595903898196,0.699583183579437));
#10152=CARTESIAN_POINT('Ctrl Pts',(4.5,-1.29087043558603,0.7));
#10153=CARTESIAN_POINT('Ctrl Pts',(4.5,-1.28575421950843,0.7));
#10154=CARTESIAN_POINT('',(4.5,-1.41772989878425,0.));
#10155=CARTESIAN_POINT('Ctrl Pts',(4.5,-1.41772989878425,0.));
#10156=CARTESIAN_POINT('Ctrl Pts',(4.5,-1.41239649634988,0.100698149937961));
#10157=CARTESIAN_POINT('Ctrl Pts',(4.5,-1.40706297966336,0.201396293824709));
#10158=CARTESIAN_POINT('Ctrl Pts',(4.5,-1.39637633579674,0.403158471769294));
#10159=CARTESIAN_POINT('Ctrl Pts',(4.5,-1.39102320777973,0.504222505781934));
#10160=CARTESIAN_POINT('Ctrl Pts',(4.5,-1.38566996325095,0.605286533624017));
#10161=CARTESIAN_POINT('',(4.5,-1.48481481481482,0.));
#10162=CARTESIAN_POINT('Origin',(1.1,-1.39290118819044,0.));
#10163=CARTESIAN_POINT('',(1.1,1.324891758307,0.));
#10164=CARTESIAN_POINT('',(1.1,-1.39290118819044,0.));
#10165=CARTESIAN_POINT('',(1.10000000295569,1.29254692766489,0.605334652628491));
#10166=CARTESIAN_POINT('Ctrl Pts',(1.10000000295569,1.29254692766489,0.605334652628491));
#10167=CARTESIAN_POINT('Ctrl Pts',(1.10000000295569,1.29794978210809,0.504228164786351));
#10168=CARTESIAN_POINT('Ctrl Pts',(1.1,1.30335245345465,0.403121008362245));
#10169=CARTESIAN_POINT('Ctrl Pts',(1.1,1.31413403739463,0.20134322693425));
#10170=CARTESIAN_POINT('Ctrl Pts',(1.1,1.31951302132877,0.100671299071668));
#10171=CARTESIAN_POINT('Ctrl Pts',(1.1,1.324891758307,0.));
#10172=CARTESIAN_POINT('Ctrl Pts',(1.1,1.19266190204553,0.7));
#10173=CARTESIAN_POINT('Ctrl Pts',(1.1,1.20057109129252,0.7));
#10174=CARTESIAN_POINT('Ctrl Pts',(1.10000046829629,1.20841685974333,0.699006220526237));
#10175=CARTESIAN_POINT('Ctrl Pts',(1.10000087277688,1.21605887983377,0.697119382842322));
#10176=CARTESIAN_POINT('Ctrl Pts',(1.10000109992184,1.22035042410288,0.696059787689036));
#10177=CARTESIAN_POINT('Ctrl Pts',(1.10000130563842,1.22457776983048,0.694717521940989));
#10178=CARTESIAN_POINT('Ctrl Pts',(1.10000143498593,1.22871439246446,0.693103507978966));
#10179=CARTESIAN_POINT('Ctrl Pts',(1.10000166711622,1.23613807995602,0.690206957744321));
#10180=CARTESIAN_POINT('Ctrl Pts',(1.10000160692769,1.24318920265812,0.686469797174223));
#10181=CARTESIAN_POINT('Ctrl Pts',(1.10000129432656,1.24972159507123,0.681973692132557));
#10182=CARTESIAN_POINT('Ctrl Pts',(1.10000112259081,1.25331033895651,0.679503636989594));
#10183=CARTESIAN_POINT('Ctrl Pts',(1.10000088087184,1.25674225826706,0.676803638555143));
#10184=CARTESIAN_POINT('Ctrl Pts',(1.10000066684112,1.25998923415267,0.673881729486736));
#10185=CARTESIAN_POINT('Ctrl Pts',(1.100000457217,1.26316935916797,0.671019978599686));
#10186=CARTESIAN_POINT('Ctrl Pts',(1.1000002715704,1.26615273734033,0.667962699881477));
#10187=CARTESIAN_POINT('Ctrl Pts',(1.1000002731257,1.2689166530284,0.664721467295484));
#10188=CARTESIAN_POINT('Ctrl Pts',(1.10000027600127,1.2740268283512,0.658728785663437));
#10189=CARTESIAN_POINT('Ctrl Pts',(1.10000085014601,1.27838972527875,0.652108677049879));
#10190=CARTESIAN_POINT('Ctrl Pts',(1.1000010530947,1.28194599975408,0.64502688444408));
#10191=CARTESIAN_POINT('Ctrl Pts',(1.10000107362034,1.2823056710724,0.644310652415237));
#10192=CARTESIAN_POINT('Ctrl Pts',(1.10000109127028,1.28265705236355,0.643589678557342));
#10193=CARTESIAN_POINT('Ctrl Pts',(1.10000110571348,1.28300005475086,0.642864123553892));
#10194=CARTESIAN_POINT('Ctrl Pts',(1.10000124853573,1.28639184812822,0.635689442715943));
#10195=CARTESIAN_POINT('Ctrl Pts',(1.10000097361067,1.28892914698194,0.628151301589031));
#10196=CARTESIAN_POINT('Ctrl Pts',(1.10000056283738,1.29055881622654,0.620418355899457));
#10197=CARTESIAN_POINT('Ctrl Pts',(1.10000029930222,1.29160434466024,0.615457217544876));
#10198=CARTESIAN_POINT('Ctrl Pts',(1.0999999999818,1.29227543558766,0.610415225971447));
#10199=CARTESIAN_POINT('Ctrl Pts',(1.1000000000255,1.29254692753179,0.605334652628598));
#10200=CARTESIAN_POINT('',(1.10000000295569,-1.29254692766489,0.605334652628491));
#10201=CARTESIAN_POINT('Ctrl Pts',(1.1000000000255,-1.29254692753179,0.605334652628598));
#10202=CARTESIAN_POINT('Ctrl Pts',(1.09999999995744,-1.29212405100831,0.613248166229861));
#10203=CARTESIAN_POINT('Ctrl Pts',(1.10000066442022,-1.29073420569755,0.621070584654331));
#10204=CARTESIAN_POINT('Ctrl Pts',(1.10000095378343,-1.28846118610397,0.628641296001913));
#10205=CARTESIAN_POINT('Ctrl Pts',(1.10000111506646,-1.28719426797524,0.632861000698125));
#10206=CARTESIAN_POINT('Ctrl Pts',(1.10000118318417,-1.28565198202118,0.637002542581089));
#10207=CARTESIAN_POINT('Ctrl Pts',(1.10000113489265,-1.28384214455607,0.641036116698538));
#10208=CARTESIAN_POINT('Ctrl Pts',(1.10000104828677,-1.28059638744501,0.648269916488365));
#10209=CARTESIAN_POINT('Ctrl Pts',(1.10000053334783,-1.27652829029495,0.655078571385522));
#10210=CARTESIAN_POINT('Ctrl Pts',(1.10000033433257,-1.27170133822839,0.661298646557671));
#10211=CARTESIAN_POINT('Ctrl Pts',(1.10000029715544,-1.27079963749419,0.662460590217389));
#10212=CARTESIAN_POINT('Ctrl Pts',(1.10000027400485,-1.26987132743055,0.663601924550879));
#10213=CARTESIAN_POINT('Ctrl Pts',(1.10000027368829,-1.26891665304159,0.664721467295481));
#10214=CARTESIAN_POINT('Ctrl Pts',(1.10000027305905,-1.2670190620795,0.666946764442229));
#10215=CARTESIAN_POINT('Ctrl Pts',(1.10000036187052,-1.26501734165944,0.669086014589825));
#10216=CARTESIAN_POINT('Ctrl Pts',(1.10000048327469,-1.26291879257262,0.671135465892351));
#10217=CARTESIAN_POINT('Ctrl Pts',(1.10000081209565,-1.25723491092676,0.676686367091516));
#10218=CARTESIAN_POINT('Ctrl Pts',(1.10000132622062,-1.25090760500066,0.68151881845922));
#10219=CARTESIAN_POINT('Ctrl Pts',(1.10000150097561,-1.24410063152763,0.68557843671136));
#10220=CARTESIAN_POINT('Ctrl Pts',(1.10000161196703,-1.2397773464179,0.688156805381407));
#10221=CARTESIAN_POINT('Ctrl Pts',(1.1000016084534,-1.23525961544019,0.690422742497405));
#10222=CARTESIAN_POINT('Ctrl Pts',(1.10000148831111,-1.23058375131837,0.692353039195786));
#10223=CARTESIAN_POINT('Ctrl Pts',(1.10000130031927,-1.22326722442338,0.695373457954986));
#10224=CARTESIAN_POINT('Ctrl Pts',(1.1000008264887,-1.21564857658641,0.697539632783775));
#10225=CARTESIAN_POINT('Ctrl Pts',(1.10000044322439,-1.20787483729518,0.698781928831272));
#10226=CARTESIAN_POINT('Ctrl Pts',(1.1000001958084,-1.20285650563037,0.6995838921283));
#10227=CARTESIAN_POINT('Ctrl Pts',(1.1,-1.19777295102175,0.7));
#10228=CARTESIAN_POINT('Ctrl Pts',(1.1,-1.19266190204553,0.7));
#10229=CARTESIAN_POINT('',(1.1,-1.324891758307,0.));
#10230=CARTESIAN_POINT('Ctrl Pts',(1.1,-1.324891758307,0.));
#10231=CARTESIAN_POINT('Ctrl Pts',(1.1,-1.3195129727271,0.10067220872632));
#10232=CARTESIAN_POINT('Ctrl Pts',(1.1,-1.31413394019217,0.201345046154956));
#10233=CARTESIAN_POINT('Ctrl Pts',(1.1,-1.30335235623932,0.40312282767794));
#10234=CARTESIAN_POINT('Ctrl Pts',(1.10000000295569,-1.29794973349953,0.504229074424201));
#10235=CARTESIAN_POINT('Ctrl Pts',(1.10000000295569,-1.29254692766489,0.605334652628491));
#10236=CARTESIAN_POINT('',(1.1,-1.39290118819044,0.));
#10237=CARTESIAN_POINT('Origin',(0.199725906950915,-1.5,-0.0104671912485888));
#10238=CARTESIAN_POINT('',(0.200274469199584,1.20659878095028,0.));
#10239=CARTESIAN_POINT('',(0.200274469199585,-0.75,0.));
#10240=CARTESIAN_POINT('',(0.231993417893744,1.17491202960101,0.605233595624295));
#10241=CARTESIAN_POINT('Ctrl Pts',(0.200274469199584,1.20659878095028,-9.43255890062389E-18));
#10242=CARTESIAN_POINT('Ctrl Pts',(0.210847451958254,1.19603647956141,0.20174452921517));
#10243=CARTESIAN_POINT('Ctrl Pts',(0.221420434855641,1.18547422886796,0.403489061077219));
#10244=CARTESIAN_POINT('Ctrl Pts',(0.231993417893744,1.17491202960101,0.605233595624295));
#10245=CARTESIAN_POINT('',(0.231993417893744,-1.17491202960101,0.605233595624295));
#10246=CARTESIAN_POINT('',(0.231993417893744,-0.75,0.605233595624295));
#10247=CARTESIAN_POINT('',(0.200274469199584,-1.20659878095028,1.38777878078145E-17));
#10248=CARTESIAN_POINT('Ctrl Pts',(0.231993417893744,-1.17491202960101,
0.605233595624295));
#10249=CARTESIAN_POINT('Ctrl Pts',(0.221420434855641,-1.18547422886796,
0.40348906107722));
#10250=CARTESIAN_POINT('Ctrl Pts',(0.210847451958254,-1.19603647956141,
0.20174452921517));
#10251=CARTESIAN_POINT('Ctrl Pts',(0.200274469199584,-1.20659878095028,
2.0491421059976E-17));
#10252=CARTESIAN_POINT('',(0.200274469199585,-0.75,0.));
#10253=CARTESIAN_POINT('Origin',(6.87299528185878,-3.57834294608796E-18,
0.));
#10254=CARTESIAN_POINT('Ctrl Pts',(8.90000000000001,-1.62420669932031,-3.75133951679985E-17));
#10255=CARTESIAN_POINT('Ctrl Pts',(10.0682843079684,-1.69891080436391,-1.31961514553165E-7));
#10256=CARTESIAN_POINT('Ctrl Pts',(11.2345361392062,-1.79243531443695,-6.44452192334729E-8));
#10257=CARTESIAN_POINT('Ctrl Pts',(12.4000000002382,-1.91212902541327,2.95121624705651E-11));
#10258=CARTESIAN_POINT('Ctrl Pts',(12.4000000002382,1.91212902541327,2.95118849063386E-11));
#10259=CARTESIAN_POINT('Ctrl Pts',(11.2345361911441,1.79243531977099,-6.4445136166539E-8));
#10260=CARTESIAN_POINT('Ctrl Pts',(10.0682843567552,1.69891080748336,-1.31958638870612E-7));
#10261=CARTESIAN_POINT('Ctrl Pts',(8.9,1.62420669932031,6.39679281766448E-17));
#10262=CARTESIAN_POINT('',(8.7,1.61160179736194,0.));
#10263=CARTESIAN_POINT('',(8.7,1.68851851851852,0.));
#10264=CARTESIAN_POINT('Ctrl Pts',(8.70000000002062,1.61160179731554,-3.21507306454832E-13));
#10265=CARTESIAN_POINT('Ctrl Pts',(7.99734938728961,1.56795839277283,5.29471456843263E-9));
#10266=CARTESIAN_POINT('Ctrl Pts',(7.29393815910572,1.53097060499506,-6.44604909847991E-9));
#10267=CARTESIAN_POINT('Ctrl Pts',(6.58949465297818,1.49904250536939,-7.60372244394637E-9));
#10268=CARTESIAN_POINT('Ctrl Pts',(5.94302350041144,1.46974193664425,-8.66612477447903E-9));
#10269=CARTESIAN_POINT('Ctrl Pts',(5.29757001768168,1.44478244743454,1.79883147367388E-8));
#10270=CARTESIAN_POINT('Ctrl Pts',(4.65216233480351,1.42284617839366,3.84107779578714E-9));
#10271=CARTESIAN_POINT('Ctrl Pts',(4.60144142975536,1.4211222642714,2.72928337404163E-9));
#10272=CARTESIAN_POINT('Ctrl Pts',(4.55072080855761,1.41941704699729,1.44770501019496E-9));
#10273=CARTESIAN_POINT('Ctrl Pts',(4.50000000001737,1.41772989873549,-1.00876616052154E-12));
#10274=CARTESIAN_POINT('',(4.3,1.41116952203211,0.));
#10275=CARTESIAN_POINT('',(4.3,1.48481481481482,0.));
#10276=CARTESIAN_POINT('Ctrl Pts',(4.3,1.41116952203211,-1.0790522121662E-15));
#10277=CARTESIAN_POINT('Ctrl Pts',(3.23514221724601,1.37672428690534,3.20725535317031E-8));
#10278=CARTESIAN_POINT('Ctrl Pts',(2.16992716239601,1.34987955958158,4.63097810372671E-9));
#10279=CARTESIAN_POINT('Ctrl Pts',(1.10000000020726,1.32489175811528,-9.82792569252214E-12));
#10280=CARTESIAN_POINT('',(0.9,1.32024227787037,0.));
#10281=CARTESIAN_POINT('',(0.9,1.39290118819044,0.));
#10282=CARTESIAN_POINT('',(0.297857995688647,1.306435779838,0.));
#10283=CARTESIAN_POINT('Ctrl Pts',(0.9,1.32024227787037,-6.93889390390723E-18));
#10284=CARTESIAN_POINT('Ctrl Pts',(0.699470323836888,1.31560060380002,-4.72996299588896E-10));
#10285=CARTESIAN_POINT('Ctrl Pts',(0.498765843889866,1.3110112408976,-1.02277582142263E-13));
#10286=CARTESIAN_POINT('Ctrl Pts',(0.297857995688647,1.306435779838,-1.00157829096748E-16));
#10287=CARTESIAN_POINT('Ctrl Pts',(0.297857995688647,1.306435779838,-1.95156391047391E-17));
#10288=CARTESIAN_POINT('Ctrl Pts',(0.289922476296638,1.30625505685688,-1.46278605970555E-13));
#10289=CARTESIAN_POINT('Ctrl Pts',(0.282050301799808,1.30510306275878,-1.25203502999379E-6));
#10290=CARTESIAN_POINT('Ctrl Pts',(0.274405144964298,1.30305953674341,-1.39678564665046E-6));
#10291=CARTESIAN_POINT('Ctrl Pts',(0.269498922713003,1.30174811919849,-1.48967827287246E-6));
#10292=CARTESIAN_POINT('Ctrl Pts',(0.26468600784495,1.30006837070384,-1.17796618578504E-6));
#10293=CARTESIAN_POINT('Ctrl Pts',(0.260012701218123,1.29803054880949,-5.63923085528507E-7));
#10294=CARTESIAN_POINT('Ctrl Pts',(0.252740988282594,1.29485967708789,3.91534262267771E-7));
#10295=CARTESIAN_POINT('Ctrl Pts',(0.245891302634708,1.2908611961912,2.26944434681222E-6));
#10296=CARTESIAN_POINT('Ctrl Pts',(0.239629152465829,1.28609427281,1.73040332626933E-6));
#10297=CARTESIAN_POINT('Ctrl Pts',(0.238677421334952,1.28536978852616,1.6484790500646E-6));
#10298=CARTESIAN_POINT('Ctrl Pts',(0.23773930716971,1.28462746803483,1.50379952206709E-6));
#10299=CARTESIAN_POINT('Ctrl Pts',(0.236815449960777,1.28386742955246,1.27686598471174E-6));
#10300=CARTESIAN_POINT('Ctrl Pts',(0.233849259515119,1.28142720517261,5.48259784756267E-7));
#10301=CARTESIAN_POINT('Ctrl Pts',(0.231029859162728,1.27880446664625,-1.01231737317126E-6));
#10302=CARTESIAN_POINT('Ctrl Pts',(0.228365947504865,1.27601569667724,-2.73789903475208E-6));
#10303=CARTESIAN_POINT('Ctrl Pts',(0.222875659368053,1.2702680771449,-6.2943009513513E-6));
#10304=CARTESIAN_POINT('Ctrl Pts',(0.218108003769119,1.26388547870891,-1.02458913084139E-5));
#10305=CARTESIAN_POINT('Ctrl Pts',(0.214119068651703,1.25703104885628,-1.16727273233865E-5));
#10306=CARTESIAN_POINT('Ctrl Pts',(0.211608035823831,1.25271618840614,-1.25709199407453E-5));
#10307=CARTESIAN_POINT('Ctrl Pts',(0.209406266788438,1.24821342134138,-1.25531979180244E-5));
#10308=CARTESIAN_POINT('Ctrl Pts',(0.207536767894457,1.24355803714115,-1.16467700682383E-5));
#10309=CARTESIAN_POINT('Ctrl Pts',(0.204585779527196,1.23620955211972,-1.02159812889057E-5));
#10310=CARTESIAN_POINT('Ctrl Pts',(0.20249437279756,1.22856635796309,-6.44823334219156E-6));
#10311=CARTESIAN_POINT('Ctrl Pts',(0.201333199355162,1.22077498745768,-3.37414558979738E-6));
#10312=CARTESIAN_POINT('Ctrl Pts',(0.200635497716839,1.21609347152911,-1.5270519663277E-6));
#10313=CARTESIAN_POINT('Ctrl Pts',(0.200274469246579,1.21135795995708,-3.76748562593766E-12));
#10314=CARTESIAN_POINT('Ctrl Pts',(0.200274469199584,1.20659878095028,6.07153216591882E-18));
#10315=CARTESIAN_POINT('',(-2.81723893694256E-19,1.20714678905882,-2.77862675945125E-17));
#10316=CARTESIAN_POINT('',(0.,-1.5,0.));
#10317=CARTESIAN_POINT('',(0.292751161823634,1.50665779898694,0.));
#10318=CARTESIAN_POINT('Ctrl Pts',(0.292751161823634,1.50665779898694,-4.77048955893622E-17));
#10319=CARTESIAN_POINT('Ctrl Pts',(0.274916014309114,1.50625165707847,3.84528327419955E-12));
#10320=CARTESIAN_POINT('Ctrl Pts',(0.257184594685611,1.50420857033458,-2.03607170333744E-6));
#10321=CARTESIAN_POINT('Ctrl Pts',(0.239764500086274,1.50063675387888,-2.79213621391921E-6));
#10322=CARTESIAN_POINT('Ctrl Pts',(0.222116086584643,1.49701812291205,-3.55811018958082E-6));
#10323=CARTESIAN_POINT('Ctrl Pts',(0.204785660682177,1.49183000356027,-2.9511242418033E-6));
#10324=CARTESIAN_POINT('Ctrl Pts',(0.187998620502071,1.4851341555102,-6.80337370794577E-7));
#10325=CARTESIAN_POINT('Ctrl Pts',(0.185044527596802,1.48395585623842,-2.80736529130144E-7));
#10326=CARTESIAN_POINT('Ctrl Pts',(0.182107319868513,1.48273075079643,1.61255976403501E-7));
#10327=CARTESIAN_POINT('Ctrl Pts',(0.17918831289364,1.48145903083089,6.35063889779883E-7));
#10328=CARTESIAN_POINT('Ctrl Pts',(0.162608037952008,1.47423552404966,3.32634402063389E-6));
#10329=CARTESIAN_POINT('Ctrl Pts',(0.146760254055949,1.46557586252388,7.36741945499403E-6));
#10330=CARTESIAN_POINT('Ctrl Pts',(0.131860714325404,1.4555643673366,8.80872142158042E-6));
#10331=CARTESIAN_POINT('Ctrl Pts',(0.12416804976458,1.45039541073654,9.55286874158632E-6));
#10332=CARTESIAN_POINT('Ctrl Pts',(0.116728404005452,1.44486529627202,9.54902993357918E-6));
#10333=CARTESIAN_POINT('Ctrl Pts',(0.109574210210226,1.43898090192647,7.86258910610491E-6));
#10334=CARTESIAN_POINT('Ctrl Pts',(0.100675189791982,1.43166137062374,5.76484451217541E-6));
#10335=CARTESIAN_POINT('Ctrl Pts',(0.0922175942578585,1.42379373777092,
1.07962821494929E-6));
#10336=CARTESIAN_POINT('Ctrl Pts',(0.0842272493232774,1.41542759110015,
-4.17082519724513E-6));
#10337=CARTESIAN_POINT('Ctrl Pts',(0.0719003514327883,1.40252093480537,
-1.22708263387205E-5));
#10338=CARTESIAN_POINT('Ctrl Pts',(0.0607923942774574,1.38854365509349,
-2.1446290640466E-5));
#10339=CARTESIAN_POINT('Ctrl Pts',(0.0509667079859164,1.37370740939602,
-2.73088451608079E-5));
#10340=CARTESIAN_POINT('Ctrl Pts',(0.040988527714452,1.35864090617899,-3.32623861267576E-5));
#10341=CARTESIAN_POINT('Ctrl Pts',(0.0323319291028794,1.34268723517955,
-3.58272570146011E-5));
#10342=CARTESIAN_POINT('Ctrl Pts',(0.0251054147216294,1.32603775378173,
-3.42048160832586E-5));
#10343=CARTESIAN_POINT('Ctrl Pts',(0.0239557673766072,1.32338903116455,
-3.39467061825833E-5));
#10344=CARTESIAN_POINT('Ctrl Pts',(0.022842414085455,1.32072266145131,-3.35898145907185E-5));
#10345=CARTESIAN_POINT('Ctrl Pts',(0.0217659098422027,1.31803938112476,
-3.31388957009043E-5));
#10346=CARTESIAN_POINT('Ctrl Pts',(0.0146851456525434,1.30038996137917,
-3.01729526055095E-5));
#10347=CARTESIAN_POINT('Ctrl Pts',(0.00925910545076598,1.282173175788,-2.28911926108039E-5));
#10348=CARTESIAN_POINT('Ctrl Pts',(0.0055880418397064,1.26361786690427,
-1.53360241296986E-5));
#10349=CARTESIAN_POINT('Ctrl Pts',(0.00217213684284492,1.24635225152695,
-8.30598038733772E-6));
#10350=CARTESIAN_POINT('Ctrl Pts',(0.000275638047107462,1.2287919996398,
-1.11502351997496E-6));
#10351=CARTESIAN_POINT('Ctrl Pts',(2.78020181985954E-5,1.21111091902543,
-1.13803743790751E-7));
#10352=CARTESIAN_POINT('Ctrl Pts',(9.289355304618E-6,1.20979019141994,-3.90154078055202E-8));
#10353=CARTESIAN_POINT('Ctrl Pts',(3.5054796412911E-11,1.20846879032832,
-2.82152417201308E-12));
#10354=CARTESIAN_POINT('Ctrl Pts',(6.5594231435373E-18,1.20714678905882,
2.42861286636753E-17));
#10355=CARTESIAN_POINT('',(12.8678148030684,2.16300527278356,0.));
#10356=CARTESIAN_POINT('Ctrl Pts',(0.292751161823634,1.50665779898694,0.));
#10357=CARTESIAN_POINT('Ctrl Pts',(4.48443904223854,1.60211086545473,0.));
#10358=CARTESIAN_POINT('Ctrl Pts',(8.67612692265345,1.70561506876628,0.));
#10359=CARTESIAN_POINT('Ctrl Pts',(12.8678148030684,2.16300527278356,0.));
#10360=CARTESIAN_POINT('',(13.2,1.86519007666192,1.29914761427265E-16));
#10361=CARTESIAN_POINT('Ctrl Pts',(13.2,1.86519007666192,1.40512601554121E-16));
#10362=CARTESIAN_POINT('Ctrl Pts',(13.2000000013352,1.88296731840607,9.35191444695304E-11));
#10363=CARTESIAN_POINT('Ctrl Pts',(13.1983511006715,1.90064589040826,-4.81925060583158E-6));
#10364=CARTESIAN_POINT('Ctrl Pts',(13.1951709302004,1.91804121845656,-9.22684518112407E-6));
#10365=CARTESIAN_POINT('Ctrl Pts',(13.1919252271695,1.93579500539423,-1.37252653764835E-5));
#10366=CARTESIAN_POINT('Ctrl Pts',(13.1870840836913,1.95325521073227,-1.77396479500911E-5));
#10367=CARTESIAN_POINT('Ctrl Pts',(13.1807207319279,1.9702167899609,-1.88895599539727E-5));
#10368=CARTESIAN_POINT('Ctrl Pts',(13.179605107926,1.97319049715201,-1.90911627380646E-5));
#10369=CARTESIAN_POINT('Ctrl Pts',(13.1784425783122,1.97614882406338,-1.92137058190342E-5));
#10370=CARTESIAN_POINT('Ctrl Pts',(13.1772333926356,1.97909058504493,-1.92562174744009E-5));
#10371=CARTESIAN_POINT('Ctrl Pts',(13.1703491364924,1.99583891121373,-1.94982490583826E-5));
#10372=CARTESIAN_POINT('Ctrl Pts',(13.1620175712498,2.0119031422279,-1.67925698753361E-5));
#10373=CARTESIAN_POINT('Ctrl Pts',(13.1523342210936,2.02708796667103,-1.30402710852334E-5));
#10374=CARTESIAN_POINT('Ctrl Pts',(13.1443502942575,2.03960786168842,-9.94649893779315E-6));
#10375=CARTESIAN_POINT('Ctrl Pts',(13.1354462980072,2.05153020544825,-6.18593217696112E-6));
#10376=CARTESIAN_POINT('Ctrl Pts',(13.1256528604983,2.06273196126272,-4.73977425690188E-6));
#10377=CARTESIAN_POINT('Ctrl Pts',(13.1217453950533,2.06720132901318,-4.16277439392992E-6));
#10378=CARTESIAN_POINT('Ctrl Pts',(13.1176961215346,2.07155579183536,-3.97575052791371E-6));
#10379=CARTESIAN_POINT('Ctrl Pts',(13.1135113749213,2.07579033931164,-3.99023031318383E-6));
#10380=CARTESIAN_POINT('Ctrl Pts',(13.1009362730034,2.08851509208914,-4.03374185458576E-6));
#10381=CARTESIAN_POINT('Ctrl Pts',(13.0872516297578,2.10004749226926,-5.60236028337187E-6));
#10382=CARTESIAN_POINT('Ctrl Pts',(13.0726646436523,2.11028882659185,-6.03124820804926E-6));
#10383=CARTESIAN_POINT('Ctrl Pts',(13.0580194031224,2.12057106059247,-6.46184893473862E-6));
#10384=CARTESIAN_POINT('Ctrl Pts',(13.0424632957183,2.12955278528135,-5.76500392338198E-6));
#10385=CARTESIAN_POINT('Ctrl Pts',(13.0261754841647,2.13709349482706,-4.98347139369932E-6));
#10386=CARTESIAN_POINT('Ctrl Pts',(13.0233759049672,2.13838960594114,-4.84914013593099E-6));
#10387=CARTESIAN_POINT('Ctrl Pts',(13.0205546633935,2.13964302898522,-4.72077764982159E-6));
#10388=CARTESIAN_POINT('Ctrl Pts',(13.0177126224567,2.14085289970554,-4.61407510358037E-6));
#10389=CARTESIAN_POINT('Ctrl Pts',(13.0148367726024,2.14207716304734,-4.50610322390289E-6));
#10390=CARTESIAN_POINT('Ctrl Pts',(13.0119432782921,2.14325527660784,-4.42172619954107E-6));
#10391=CARTESIAN_POINT('Ctrl Pts',(13.0090331608036,2.14438664763146,-4.38057543634576E-6));
#10392=CARTESIAN_POINT('Ctrl Pts',(12.9922536897216,2.1509100294015,-4.14330390220891E-6));
#10393=CARTESIAN_POINT('Ctrl Pts',(12.9749229882599,2.15588345271621,-5.05640020348117E-6));
#10394=CARTESIAN_POINT('Ctrl Pts',(12.9572550825995,2.15928949382789,-4.85686529648217E-6));
#10395=CARTESIAN_POINT('Ctrl Pts',(12.9529252316797,2.16012420794307,-4.80796553341985E-6));
#10396=CARTESIAN_POINT('Ctrl Pts',(12.9485750628159,2.16086455090717,-4.70814629363608E-6));
#10397=CARTESIAN_POINT('Ctrl Pts',(12.944207640703,2.16150979950679,-4.55317442353944E-6));
#10398=CARTESIAN_POINT('Ctrl Pts',(12.9263774359968,2.16414405704371,-3.92049452767182E-6));
#10399=CARTESIAN_POINT('Ctrl Pts',(12.9083632163621,2.16518216214944,-2.15504024707585E-6));
#10400=CARTESIAN_POINT('Ctrl Pts',(12.8903762705535,2.16459816844574,-9.12104093693782E-7));
#10401=CARTESIAN_POINT('Ctrl Pts',(12.8828459063217,2.16435367528137,-3.91739933400607E-7));
#10402=CARTESIAN_POINT('Ctrl Pts',(12.8753202361859,2.1638242536466,5.87463683432524E-12));
#10403=CARTESIAN_POINT('Ctrl Pts',(12.8678148030684,2.16300527278357,2.8796409701215E-16));
#10404=CARTESIAN_POINT('',(13.2,-1.86519007666192,1.11326398357188E-16));
#10405=CARTESIAN_POINT('',(13.2,2.2,0.));
#10406=CARTESIAN_POINT('',(12.8678148030684,-2.16300527278356,1.38777878078145E-17));
#10407=CARTESIAN_POINT('Ctrl Pts',(12.8678148030684,-2.16300527278357,2.56739074444567E-16));
#10408=CARTESIAN_POINT('Ctrl Pts',(12.8854929372559,-2.16493428409685,8.24591542686399E-11));
#10409=CARTESIAN_POINT('Ctrl Pts',(12.9032520674897,-2.16521372082443,-4.52295339524789E-6));
#10410=CARTESIAN_POINT('Ctrl Pts',(12.9208958607904,-2.1639404182545,-8.68231213275745E-6));
#10411=CARTESIAN_POINT('Ctrl Pts',(12.9389012534027,-2.16264102008682,-1.29269145154966E-5));
#10412=CARTESIAN_POINT('Ctrl Pts',(12.9567880250381,-2.15972433317902,-1.67278855193166E-5));
#10413=CARTESIAN_POINT('Ctrl Pts',(12.9743443410528,-2.15524079327399,-1.78237954457702E-5));
#10414=CARTESIAN_POINT('Ctrl Pts',(12.9774431846623,-2.15444940919484,-1.80172331504298E-5));
#10415=CARTESIAN_POINT('Ctrl Pts',(12.9805316913262,-2.15360908525727,-1.81351031595367E-5));
#10416=CARTESIAN_POINT('Ctrl Pts',(12.9836086301392,-2.15271994254544,-1.81766625580856E-5));
#10417=CARTESIAN_POINT('Ctrl Pts',(13.0010041030966,-2.14769317440371,-1.84116186093898E-5));
#10418=CARTESIAN_POINT('Ctrl Pts',(13.017876958431,-2.14115457229109,-1.5854618169158E-5));
#10419=CARTESIAN_POINT('Ctrl Pts',(13.0340226638693,-2.13317744288338,-1.23136839993165E-5));
#10420=CARTESIAN_POINT('Ctrl Pts',(13.0473215411186,-2.12660684953271,-9.39709115965876E-6));
#10421=CARTESIAN_POINT('Ctrl Pts',(13.060127470267,-2.11905920305061,-5.85016632862467E-6));
#10422=CARTESIAN_POINT('Ctrl Pts',(13.0723151314263,-2.11055132433008,-4.53327195050794E-6));
#10423=CARTESIAN_POINT('Ctrl Pts',(13.0772147086919,-2.10713106111368,-4.00386555564548E-6));
#10424=CARTESIAN_POINT('Ctrl Pts',(13.0820141951123,-2.10355537352593,-3.85636210984559E-6));
#10425=CARTESIAN_POINT('Ctrl Pts',(13.0867078006727,-2.0998301147952,-3.90248451975241E-6));
#10426=CARTESIAN_POINT('Ctrl Pts',(13.1007249787291,-2.08870484782034,-4.04022639510273E-6));
#10427=CARTESIAN_POINT('Ctrl Pts',(13.1136765748478,-2.07634683247102,-5.5945154994439E-6));
#10428=CARTESIAN_POINT('Ctrl Pts',(13.1254414850725,-2.06295113861397,-5.97495381195624E-6));
#10429=CARTESIAN_POINT('Ctrl Pts',(13.1372476314214,-2.04950849272046,-6.35672556443159E-6));
#10430=CARTESIAN_POINT('Ctrl Pts',(13.1478597809499,-2.03501968083851,-5.56609061204695E-6));
#10431=CARTESIAN_POINT('Ctrl Pts',(13.1571184147632,-2.01964723728874,-4.75455255839871E-6));
#10432=CARTESIAN_POINT('Ctrl Pts',(13.158708901902,-2.01700649414547,-4.61514313115074E-6));
#10433=CARTESIAN_POINT('Ctrl Pts',(13.1602593369672,-2.01433961799121,-4.48389992381974E-6));
#10434=CARTESIAN_POINT('Ctrl Pts',(13.1617687665475,-2.01164737048868,-4.37752847101542E-6));
#10435=CARTESIAN_POINT('Ctrl Pts',(13.1632768494098,-2.00895752501823,-4.27125192317111E-6));
#10436=CARTESIAN_POINT('Ctrl Pts',(13.164742106841,-2.00624572954308,-4.19089851494128E-6));
#10437=CARTESIAN_POINT('Ctrl Pts',(13.1661638648313,-2.00351289682408,-4.15637526360595E-6));
#10438=CARTESIAN_POINT('Ctrl Pts',(13.1744716670281,-1.98754405133797,-3.95464448717833E-6));
#10439=CARTESIAN_POINT('Ctrl Pts',(13.181298057795,-1.97085874357403,-5.01850453361653E-6));
#10440=CARTESIAN_POINT('Ctrl Pts',(13.1866022393826,-1.95366776591112,-4.89891140766866E-6));
#10441=CARTESIAN_POINT('Ctrl Pts',(13.1879075264936,-1.94943729958961,-4.86948116225E-6));
#10442=CARTESIAN_POINT('Ctrl Pts',(13.1891204013114,-1.94517611908519,-4.78523710928743E-6));
#10443=CARTESIAN_POINT('Ctrl Pts',(13.1902397948733,-1.94088722910442,-4.64104147683466E-6));
#10444=CARTESIAN_POINT('Ctrl Pts',(13.1947901580114,-1.92345278286841,-4.05488258426869E-6));
#10445=CARTESIAN_POINT('Ctrl Pts',(13.1977733658442,-1.90566244769967,-2.24449026644408E-6));
#10446=CARTESIAN_POINT('Ctrl Pts',(13.1991406030032,-1.88772335428786,-9.50757284845071E-7));
#10447=CARTESIAN_POINT('Ctrl Pts',(13.1997114533543,-1.8802334044254,-4.10596478211383E-7));
#10448=CARTESIAN_POINT('Ctrl Pts',(13.2000000000958,-1.87271737110067,6.9401096738129E-12));
#10449=CARTESIAN_POINT('Ctrl Pts',(13.2,-1.86519007666192,1.81278603239576E-16));
#10450=CARTESIAN_POINT('',(0.292751161823634,-1.50665779898694,-1.38777878078145E-17));
#10451=CARTESIAN_POINT('Ctrl Pts',(12.8678148030684,-2.16300527278356,0.));
#10452=CARTESIAN_POINT('Ctrl Pts',(8.67612692265345,-1.70561506876628,0.));
#10453=CARTESIAN_POINT('Ctrl Pts',(4.48443904223854,-1.60211086545473,0.));
#10454=CARTESIAN_POINT('Ctrl Pts',(0.292751161823634,-1.50665779898694,
0.));
#10455=CARTESIAN_POINT('',(4.02814324098787E-18,-1.20714678905882,5.54818711994559E-17));
#10456=CARTESIAN_POINT('Ctrl Pts',(-2.22044604925031E-16,-1.20714678905882,
-3.98986399474666E-17));
#10457=CARTESIAN_POINT('Ctrl Pts',(2.12382277713531E-10,-1.2249878157372,
-1.35440422383976E-12));
#10458=CARTESIAN_POINT('Ctrl Pts',(0.00163882612763064,-1.24276245549475,
-1.96699749426327E-6));
#10459=CARTESIAN_POINT('Ctrl Pts',(0.00481304415265273,-1.26026068126938,
-2.66007142975038E-6));
#10460=CARTESIAN_POINT('Ctrl Pts',(0.00802873944670128,-1.27798755504872,
-3.36220171040687E-6));
#10461=CARTESIAN_POINT('Ctrl Pts',(0.0128206026099745,-1.29543230475431,
-2.69550948014298E-6));
#10462=CARTESIAN_POINT('Ctrl Pts',(0.0191320595672371,-1.31236817798419,
-4.00401478067381E-7));
#10463=CARTESIAN_POINT('Ctrl Pts',(0.0202443702650641,-1.31535290133701,
4.0809101773195E-9));
#10464=CARTESIAN_POINT('Ctrl Pts',(0.0214039964883031,-1.3183217636574,
4.5005107558061E-7));
#10465=CARTESIAN_POINT('Ctrl Pts',(0.0226107760969305,-1.32127343934773,
9.26779280916758E-7));
#10466=CARTESIAN_POINT('Ctrl Pts',(0.0294548697216842,-1.33801348419941,
3.63048130534217E-6));
#10467=CARTESIAN_POINT('Ctrl Pts',(0.0377511831708778,-1.35405403406083,
7.64722139837078E-6));
#10468=CARTESIAN_POINT('Ctrl Pts',(0.0474204318104353,-1.36917746582299,
9.03443059383348E-6));
#10469=CARTESIAN_POINT('Ctrl Pts',(0.0524109755304394,-1.37698305136733,
9.75040433665629E-6));
#10470=CARTESIAN_POINT('Ctrl Pts',(0.0577680562174045,-1.38454410063597,
9.71159147480002E-6));
#10471=CARTESIAN_POINT('Ctrl Pts',(0.0634855547170043,-1.39182806229354,
7.98761394269614E-6));
#10472=CARTESIAN_POINT('Ctrl Pts',(0.0706048733905122,-1.40089791062835,
5.84095042579577E-6));
#10473=CARTESIAN_POINT('Ctrl Pts',(0.0782829434694699,-1.40953838460506,
1.09773645972912E-6));
#10474=CARTESIAN_POINT('Ctrl Pts',(0.0864706998703675,-1.41772246232928,
-4.21049985396393E-6));
#10475=CARTESIAN_POINT('Ctrl Pts',(0.0990944981487371,-1.43034058886193,
-1.2394683793612E-5));
#10476=CARTESIAN_POINT('Ctrl Pts',(0.112816484288725,-1.44176429483685,
-2.16481703631134E-5));
#10477=CARTESIAN_POINT('Ctrl Pts',(0.127426518150943,-1.45192534842919,
-2.7562374581111E-5));
#10478=CARTESIAN_POINT('Ctrl Pts',(0.142261949549145,-1.46224316253723,
-3.35678206860622E-5));
#10479=CARTESIAN_POINT('Ctrl Pts',(0.158014355623482,-1.47125989363127,
-3.6155642403295E-5));
#10480=CARTESIAN_POINT('Ctrl Pts',(0.17449494651519,-1.47886261331763,-3.45187637154371E-5));
#10481=CARTESIAN_POINT('Ctrl Pts',(0.177115379630184,-1.48007145458801,
-3.42584981007467E-5));
#10482=CARTESIAN_POINT('Ctrl Pts',(0.179754261386328,-1.48124444832217,
-3.38986806574493E-5));
#10483=CARTESIAN_POINT('Ctrl Pts',(0.18241086941249,-1.48238102342202,-3.34441145409493E-5));
#10484=CARTESIAN_POINT('Ctrl Pts',(0.199890279181845,-1.48985922935543,
-3.04532527580594E-5));
#10485=CARTESIAN_POINT('Ctrl Pts',(0.217974246898519,-1.49569663469242,
-2.31073027206853E-5));
#10486=CARTESIAN_POINT('Ctrl Pts',(0.236436446036386,-1.49978781870256,
-1.54828395726751E-5));
#10487=CARTESIAN_POINT('Ctrl Pts',(0.253618559172887,-1.50359533838099,
-8.38702246898572E-6));
#10488=CARTESIAN_POINT('Ctrl Pts',(0.271129804961754,-1.50589051664322,
-1.1237837803371E-6));
#10489=CARTESIAN_POINT('Ctrl Pts',(0.288799387895208,-1.50654014509364,
-1.14426782679271E-7));
#10490=CARTESIAN_POINT('Ctrl Pts',(0.290115790923368,-1.5065885431154,-3.92285953074499E-8));
#10491=CARTESIAN_POINT('Ctrl Pts',(0.291433072638222,-1.50662778343727,
-2.32210426557352E-12));
#10492=CARTESIAN_POINT('Ctrl Pts',(0.292751161823634,-1.50665779898694,
2.86229373536173E-17));
#10493=CARTESIAN_POINT('',(0.,-1.5,0.));
#10494=CARTESIAN_POINT('',(0.297857995688647,-1.306435779838,0.));
#10495=CARTESIAN_POINT('Ctrl Pts',(0.200274469199585,-1.20659878095028,
-5.63785129692462E-18));
#10496=CARTESIAN_POINT('Ctrl Pts',(0.200274469233139,-1.21453676310593,
-8.71436967499621E-13));
#10497=CARTESIAN_POINT('Ctrl Pts',(0.201246859971722,-1.22243356087926,
-1.21395871814677E-6));
#10498=CARTESIAN_POINT('Ctrl Pts',(0.203115675186186,-1.23012372049816,
-1.3343733317444E-6));
#10499=CARTESIAN_POINT('Ctrl Pts',(0.204315340901654,-1.23506033529553,
-1.41167219064517E-6));
#10500=CARTESIAN_POINT('Ctrl Pts',(0.20588557457721,-1.23991201018842,-1.08820351238587E-6));
#10501=CARTESIAN_POINT('Ctrl Pts',(0.207817175189242,-1.24463217458037,
-4.7123943162984E-7));
#10502=CARTESIAN_POINT('Ctrl Pts',(0.210821635148072,-1.25197403646754,
4.8840194822981E-7));
#10503=CARTESIAN_POINT('Ctrl Pts',(0.214662962735955,-1.25891288736431,
2.34840446672759E-6));
#10504=CARTESIAN_POINT('Ctrl Pts',(0.219285851586231,-1.26528190572196,
1.77850405974346E-6));
#10505=CARTESIAN_POINT('Ctrl Pts',(0.219987799701267,-1.26624898941694,
1.69196931287913E-6));
#10506=CARTESIAN_POINT('Ctrl Pts',(0.220707854727247,-1.26720289123473,
1.54254180957111E-6));
#10507=CARTESIAN_POINT('Ctrl Pts',(0.221445913570039,-1.26814297034805,
1.31084431541716E-6));
#10508=CARTESIAN_POINT('Ctrl Pts',(0.223819423285066,-1.27116615329633,
5.65732650279818E-7));
#10509=CARTESIAN_POINT('Ctrl Pts',(0.226378993511503,-1.27404655624932,
-1.0141799309673E-6));
#10510=CARTESIAN_POINT('Ctrl Pts',(0.229108317341547,-1.27677508245113,
-2.75886047820546E-6));
#10511=CARTESIAN_POINT('Ctrl Pts',(0.234729699316268,-1.28239482161129,
-6.35224711555937E-6));
#10512=CARTESIAN_POINT('Ctrl Pts',(0.241002345945823,-1.28730653457646,
-1.03364935932408E-5));
#10513=CARTESIAN_POINT('Ctrl Pts',(0.247764463424355,-1.29145035967733,
-1.17765252099068E-5));
#10514=CARTESIAN_POINT('Ctrl Pts',(0.25202072563572,-1.29405859685204,-1.26829206064147E-5));
#10515=CARTESIAN_POINT('Ctrl Pts',(0.25647185453211,-1.29636195369988,-1.26655904667795E-5));
#10516=CARTESIAN_POINT('Ctrl Pts',(0.261083107941716,-1.29833661269995,
-1.17517412599227E-5));
#10517=CARTESIAN_POINT('Ctrl Pts',(0.268362152520619,-1.30145368947124,
-1.0309194402435E-5));
#10518=CARTESIAN_POINT('Ctrl Pts',(0.275955349537693,-1.30371808689536,
-6.50743389458559E-6));
#10519=CARTESIAN_POINT('Ctrl Pts',(0.283717840216357,-1.30505580179168,
-3.40467605837577E-6));
#10520=CARTESIAN_POINT('Ctrl Pts',(0.288379557365255,-1.3058591584372,-1.54133347766382E-6));
#10521=CARTESIAN_POINT('Ctrl Pts',(0.293102847896135,-1.30632748638856,
-3.09915230996644E-12));
#10522=CARTESIAN_POINT('Ctrl Pts',(0.297857995688647,-1.306435779838,2.90566182226115E-17));
#10523=CARTESIAN_POINT('',(0.9,-1.32024227787037,0.));
#10524=CARTESIAN_POINT('Ctrl Pts',(0.297857995688651,-1.306435779838,-5.81335652359571E-17));
#10525=CARTESIAN_POINT('Ctrl Pts',(0.498765834064439,-1.31101124067384,
-1.02216845336465E-13));
#10526=CARTESIAN_POINT('Ctrl Pts',(0.699470314209512,-1.31560060357718,
-4.73070532165219E-10));
#10527=CARTESIAN_POINT('Ctrl Pts',(0.9,-1.32024227787037,4.62320796019307E-17));
#10528=CARTESIAN_POINT('',(0.9,1.39290118819044,0.));
#10529=CARTESIAN_POINT('',(4.3,-1.41116952203211,0.));
#10530=CARTESIAN_POINT('Ctrl Pts',(1.10000000020724,-1.32489175811528,-9.82782277325449E-12));
#10531=CARTESIAN_POINT('Ctrl Pts',(2.16992692797068,-1.34987955410658,4.63225598025733E-9));
#10532=CARTESIAN_POINT('Ctrl Pts',(3.23514201430925,-1.37672428034078,3.20747301048384E-8));
#10533=CARTESIAN_POINT('Ctrl Pts',(4.3,-1.41116952203211,-8.74629427996717E-16));
#10534=CARTESIAN_POINT('',(4.3,1.48481481481482,0.));
#10535=CARTESIAN_POINT('',(8.7,-1.61160179736194,0.));
#10536=CARTESIAN_POINT('Ctrl Pts',(4.50000000001737,-1.41772989873549,-1.00870158580013E-12));
#10537=CARTESIAN_POINT('Ctrl Pts',(5.14541122039116,-1.43919849219739,1.84287460122322E-8));
#10538=CARTESIAN_POINT('Ctrl Pts',(5.79079200637672,-1.46358894290692,-2.29215846350395E-9));
#10539=CARTESIAN_POINT('Ctrl Pts',(6.43711407552466,-1.49221504703413,-7.12038357450289E-9));
#10540=CARTESIAN_POINT('Ctrl Pts',(6.48784335049204,-1.49446188584227,-7.49934689782436E-9));
#10541=CARTESIAN_POINT('Ctrl Pts',(6.5385784252675,-1.49673484630497,-7.6873350528488E-9));
#10542=CARTESIAN_POINT('Ctrl Pts',(6.58931977021612,-1.49903457911226,-7.60400982311631E-9));
#10543=CARTESIAN_POINT('Ctrl Pts',(7.29382172663923,-1.5309644828944,-6.44710735180711E-9));
#10544=CARTESIAN_POINT('Ctrl Pts',(7.99729122590638,-1.56795478022256,5.29179522587699E-9));
#10545=CARTESIAN_POINT('Ctrl Pts',(8.70000000002062,-1.61160179731554,-3.21479112539667E-13));
#10546=CARTESIAN_POINT('',(8.7,1.68851851851852,0.));
#10547=CARTESIAN_POINT('',(12.6,-1.93292824674167,0.));
#10548=CARTESIAN_POINT('',(12.8889963716306,-1.96391015057091,0.));
#10549=CARTESIAN_POINT('Ctrl Pts',(12.6000000004653,-1.93292824679067,-1.00288700954909E-16));
#10550=CARTESIAN_POINT('Ctrl Pts',(12.6963367945484,-1.94307238002033,2.28133307867826E-10));
#10551=CARTESIAN_POINT('Ctrl Pts',(12.7926686848896,-1.9533982851754,-5.07154825701885E-13));
#10552=CARTESIAN_POINT('Ctrl Pts',(12.8889963716306,-1.96391015057091,2.24786696790336E-16));
#10553=CARTESIAN_POINT('',(12.9997255308004,-1.86463850151065,-1.38777878078145E-17));
#10554=CARTESIAN_POINT('Ctrl Pts',(12.8889963716306,-1.96391015057091,5.29090660172926E-17));
#10555=CARTESIAN_POINT('Ctrl Pts',(12.8968843421745,-1.96477093437063,1.28387508960266E-11));
#10556=CARTESIAN_POINT('Ctrl Pts',(12.9048206871516,-1.96464841285931,-2.5989605143924E-6));
#10557=CARTESIAN_POINT('Ctrl Pts',(12.9126487282508,-1.9636130141884,-4.24292438262167E-6));
#10558=CARTESIAN_POINT('Ctrl Pts',(12.9176900487482,-1.96294620923983,-5.30165014054907E-6));
#10559=CARTESIAN_POINT('Ctrl Pts',(12.9226867577298,-1.96189962975099,-6.00943773338864E-6));
#10560=CARTESIAN_POINT('Ctrl Pts',(12.9275953864907,-1.96048085896027,-6.09358828708331E-6));
#10561=CARTESIAN_POINT('Ctrl Pts',(12.9352257743335,-1.95827540160737,-6.22439902734509E-6));
#10562=CARTESIAN_POINT('Ctrl Pts',(12.9425549137553,-1.95519874430406,-4.64402662178521E-6));
#10563=CARTESIAN_POINT('Ctrl Pts',(12.949425376669,-1.9513005478593,-3.15156624759025E-6));
#10564=CARTESIAN_POINT('Ctrl Pts',(12.9520760960011,-1.94979656991686,-2.57575445499556E-6));
#10565=CARTESIAN_POINT('Ctrl Pts',(12.9546583803074,-1.94816978416017,-2.04880625960079E-6));
#10566=CARTESIAN_POINT('Ctrl Pts',(12.9571622133441,-1.9464211898676,-1.82278374303809E-6));
#10567=CARTESIAN_POINT('Ctrl Pts',(12.9587955877505,-1.9452804951316,-1.67533805140214E-6));
#10568=CARTESIAN_POINT('Ctrl Pts',(12.9603955609302,-1.94408794089591,-1.65796127395168E-6));
#10569=CARTESIAN_POINT('Ctrl Pts',(12.9619602112942,-1.94284549575182,-1.70649031798611E-6));
#10570=CARTESIAN_POINT('Ctrl Pts',(12.9681665721336,-1.93791719798967,-1.89898620422551E-6));
#10571=CARTESIAN_POINT('Ctrl Pts',(12.9737470546445,-1.93226498850035,-2.8025064238469E-6));
#10572=CARTESIAN_POINT('Ctrl Pts',(12.9786034821464,-1.926037248212,-2.79230211737029E-6));
#10573=CARTESIAN_POINT('Ctrl Pts',(12.9817011960737,-1.92206483066456,-2.78579321297956E-6));
#10574=CARTESIAN_POINT('Ctrl Pts',(12.9845038017717,-1.91785723501915,-2.48811564693169E-6));
#10575=CARTESIAN_POINT('Ctrl Pts',(12.9869771252785,-1.91344616543364,-2.2918341012218E-6));
#10576=CARTESIAN_POINT('Ctrl Pts',(12.9874796596041,-1.91254991636901,-2.25195326317628E-6));
#10577=CARTESIAN_POINT('Ctrl Pts',(12.9879679417815,-1.9116463809131,-2.21866365029432E-6));
#10578=CARTESIAN_POINT('Ctrl Pts',(12.98844174868,-1.91073586520696,-2.19841011183313E-6));
#10579=CARTESIAN_POINT('Ctrl Pts',(12.9918929665356,-1.9041036526468,-2.05088297829219E-6));
#10580=CARTESIAN_POINT('Ctrl Pts',(12.9945793344589,-1.89710244289626,-2.35789128083535E-6));
#10581=CARTESIAN_POINT('Ctrl Pts',(12.9964698429198,-1.88986530397042,-1.93853625224654E-6));
#10582=CARTESIAN_POINT('Ctrl Pts',(12.9984668213505,-1.88222058265133,-1.49556391743615E-6));
#10583=CARTESIAN_POINT('Ctrl Pts',(12.9995610814633,-1.87437060764114,-2.4459616079733E-7));
#10584=CARTESIAN_POINT('Ctrl Pts',(12.9997084424383,-1.86646992060833,-2.60951667192209E-8));
#10585=CARTESIAN_POINT('Ctrl Pts',(12.9997198235207,-1.86585972940924,-9.21975031242219E-9));
#10586=CARTESIAN_POINT('Ctrl Pts',(12.9997255308031,-1.86524923282631,2.14479566203628E-13));
#10587=CARTESIAN_POINT('Ctrl Pts',(12.9997255308004,-1.86463850151065,-9.54097911787244E-18));
#10588=CARTESIAN_POINT('',(12.9997255308004,1.86463850151064,1.38777878078145E-17));
#10589=CARTESIAN_POINT('',(12.9997255308004,1.1,0.));
#10590=CARTESIAN_POINT('',(12.8889963716306,1.96391015057091,0.));
#10591=CARTESIAN_POINT('Ctrl Pts',(12.9997255308004,1.86463850151065,-9.97465998686664E-18));
#10592=CARTESIAN_POINT('Ctrl Pts',(12.9997255309996,1.87257112921612,1.42345874390777E-11));
#10593=CARTESIAN_POINT('Ctrl Pts',(12.9987425107347,1.88044501776258,-2.76622459581243E-6));
#10594=CARTESIAN_POINT('Ctrl Pts',(12.9968635501128,1.8881121101061,-4.50602169498049E-6));
#10595=CARTESIAN_POINT('Ctrl Pts',(12.9956551765012,1.89304287446485,-5.62489820561454E-6));
#10596=CARTESIAN_POINT('Ctrl Pts',(12.994075066483,1.89788828888188,-6.37205869803057E-6));
#10597=CARTESIAN_POINT('Ctrl Pts',(12.9921354490207,1.90260616696402,-6.45954116508302E-6));
#10598=CARTESIAN_POINT('Ctrl Pts',(12.9891151690915,1.90995262200289,-6.59576469602218E-6));
#10599=CARTESIAN_POINT('Ctrl Pts',(12.9852608829945,1.91690476599405,-4.92589918404109E-6));
#10600=CARTESIAN_POINT('Ctrl Pts',(12.9806393828366,1.92331154882078,-3.3382766296878E-6));
#10601=CARTESIAN_POINT('Ctrl Pts',(12.9788533632605,1.92578750666072,-2.72472586378502E-6));
#10602=CARTESIAN_POINT('Ctrl Pts',(12.9769522584487,1.92818179997524,-2.1610482659023E-6));
#10603=CARTESIAN_POINT('Ctrl Pts',(12.9749381758772,1.93048453804291,-1.90960564360578E-6));
#10604=CARTESIAN_POINT('Ctrl Pts',(12.9736352090466,1.93197424425657,-1.74694031832382E-6));
#10605=CARTESIAN_POINT('Ctrl Pts',(12.9722849384098,1.93342561524533,-1.71698229815602E-6));
#10606=CARTESIAN_POINT('Ctrl Pts',(12.9708894910408,1.9348369915754,-1.75552529092739E-6));
#10607=CARTESIAN_POINT('Ctrl Pts',(12.9653179015399,1.94047218048862,-1.90941553332435E-6));
#10608=CARTESIAN_POINT('Ctrl Pts',(12.9590944588136,1.94540670303376,-2.83773366290493E-6));
#10609=CARTESIAN_POINT('Ctrl Pts',(12.9523775255978,1.94955941520082,-2.8574013135715E-6));
#10610=CARTESIAN_POINT('Ctrl Pts',(12.9480923984168,1.95220867479748,-2.86994846593266E-6));
#10611=CARTESIAN_POINT('Ctrl Pts',(12.9436054681019,1.95453912223498,-2.59559485065602E-6));
#10612=CARTESIAN_POINT('Ctrl Pts',(12.9389519978263,1.95652032281755,-2.39773084743613E-6));
#10613=CARTESIAN_POINT('Ctrl Pts',(12.9379934875219,1.95692840561619,-2.35697530915642E-6));
#10614=CARTESIAN_POINT('Ctrl Pts',(12.9370291206935,1.95732112306527,-2.32193094846859E-6));
#10615=CARTESIAN_POINT('Ctrl Pts',(12.9360592398442,1.95769827921557,-2.29894501965994E-6));
#10616=CARTESIAN_POINT('Ctrl Pts',(12.929096105975,1.96040602292032,-2.13392052256244E-6));
#10617=CARTESIAN_POINT('Ctrl Pts',(12.9218497638689,1.96231496375013,-2.36509085467933E-6));
#10618=CARTESIAN_POINT('Ctrl Pts',(12.9144555496645,1.96340894166242,-1.92146179377921E-6));
#10619=CARTESIAN_POINT('Ctrl Pts',(12.9066371708262,1.96456567495722,-1.45238421961943E-6));
#10620=CARTESIAN_POINT('Ctrl Pts',(12.8987125532455,1.96480297730229,-2.37321368026999E-7));
#10621=CARTESIAN_POINT('Ctrl Pts',(12.8908401755085,1.96409377829808,-2.55627471131237E-8));
#10622=CARTESIAN_POINT('Ctrl Pts',(12.89022523009,1.96403837970149,-9.02136684357828E-9));
#10623=CARTESIAN_POINT('Ctrl Pts',(12.8896106033158,1.96397717928728,1.9621770460073E-13));
#10624=CARTESIAN_POINT('Ctrl Pts',(12.8889963716306,1.96391015057091,-3.29597460435593E-17));
#10625=CARTESIAN_POINT('',(12.6,1.93292824674167,0.));
#10626=CARTESIAN_POINT('Ctrl Pts',(12.8889963716306,1.96391015057091,8.95144418658345E-17));
#10627=CARTESIAN_POINT('Ctrl Pts',(12.7926686852738,1.95339828521733,-5.07275478770449E-13));
#10628=CARTESIAN_POINT('Ctrl Pts',(12.6963367949308,1.94307238006059,2.28132759158623E-10));
#10629=CARTESIAN_POINT('Ctrl Pts',(12.6000000004652,1.93292824679066,-1.5019386425618E-16));
#10630=CARTESIAN_POINT('',(12.6,-1.99376954809806,0.));
#10631=CARTESIAN_POINT('Origin',(11.2,0.,0.));
#10632=CARTESIAN_POINT('',(10.8,-4.89858719658942E-17,0.7));
#10633=CARTESIAN_POINT('Origin',(11.2,0.,0.7));
#10634=CARTESIAN_POINT('',(10.8,-4.89858719658942E-17,0.));
#10635=CARTESIAN_POINT('Origin',(2.,0.,0.));
#10636=CARTESIAN_POINT('',(1.6,-4.89858719658941E-17,0.));
#10637=CARTESIAN_POINT('Origin',(12.6,-1.99376954809806,0.));
#10638=CARTESIAN_POINT('',(12.6,-1.90428042248893,0.60470250816874));
#10639=CARTESIAN_POINT('Ctrl Pts',(12.6,-1.93292824674167,0.));
#10640=CARTESIAN_POINT('Ctrl Pts',(12.6,-1.92814118331811,0.100975624959503));
#10641=CARTESIAN_POINT('Ctrl Pts',(12.6,-1.9233557423333,0.20195205683881));
#10642=CARTESIAN_POINT('Ctrl Pts',(12.6,-1.91380649287245,0.40351907263528));
#10643=CARTESIAN_POINT('Ctrl Pts',(12.6,-1.90904260275794,0.504111110768618));
#10644=CARTESIAN_POINT('Ctrl Pts',(12.6,-1.90428042248893,0.60470250816874));
#10645=CARTESIAN_POINT('',(12.6,1.90428042248893,0.60470250816874));
#10646=CARTESIAN_POINT('Ctrl Pts',(12.6,1.90428042248893,0.60470250816874));
#10647=CARTESIAN_POINT('Ctrl Pts',(12.6,1.90904310126474,0.504100580823831));
#10648=CARTESIAN_POINT('Ctrl Pts',(12.6,1.91380749024866,0.403498012513773));
#10649=CARTESIAN_POINT('Ctrl Pts',(12.6,1.92335674041114,0.201930996640285));
#10650=CARTESIAN_POINT('Ctrl Pts',(12.6,1.92814168252712,0.100965094925255));
#10651=CARTESIAN_POINT('Ctrl Pts',(12.6,1.93292824674167,0.));
#10652=CARTESIAN_POINT('',(12.6,1.80383022254432,0.7));
#10653=CARTESIAN_POINT('Ctrl Pts',(12.6,1.80383022254432,0.7));
#10654=CARTESIAN_POINT('Ctrl Pts',(12.6,1.81177675668304,0.7));
#10655=CARTESIAN_POINT('Ctrl Pts',(12.6000021803669,1.81966206665253,0.699006623620781));
#10656=CARTESIAN_POINT('Ctrl Pts',(12.6000040789681,1.8273451885609,0.69711902809518));
#10657=CARTESIAN_POINT('Ctrl Pts',(12.6000050614635,1.8313210797205,0.696142227980247));
#10658=CARTESIAN_POINT('Ctrl Pts',(12.6000059683507,1.83524283435206,0.694925046992878));
#10659=CARTESIAN_POINT('Ctrl Pts',(12.6000066021136,1.83908960013903,0.693475985595303));
#10660=CARTESIAN_POINT('Ctrl Pts',(12.6000078338507,1.84656590463324,0.690659691378536));
#10661=CARTESIAN_POINT('Ctrl Pts',(12.6000078244032,1.85367932786264,0.687000939374075));
#10662=CARTESIAN_POINT('Ctrl Pts',(12.6000065509639,1.86028396908448,0.682580904467878));
#10663=CARTESIAN_POINT('Ctrl Pts',(12.600005740321,1.86448833536622,0.679767209507086));
#10664=CARTESIAN_POINT('Ctrl Pts',(12.6000044390918,1.86848632867783,0.676643963831362));
#10665=CARTESIAN_POINT('Ctrl Pts',(12.6000033339006,1.8722338275817,0.673223162566374));
#10666=CARTESIAN_POINT('Ctrl Pts',(12.6000024442799,1.87525036668517,0.670469597843409));
#10667=CARTESIAN_POINT('Ctrl Pts',(12.600001679327,1.8780865799519,0.667539409933064));
#10668=CARTESIAN_POINT('Ctrl Pts',(12.600001676908,1.88072259809992,0.664442334323256));
#10669=CARTESIAN_POINT('Ctrl Pts',(12.6000016722164,1.88583495965423,0.658435786041233));
#10670=CARTESIAN_POINT('Ctrl Pts',(12.6000042182276,1.89019731592974,0.651802923597933));
#10671=CARTESIAN_POINT('Ctrl Pts',(12.6000050838539,1.89374834224248,0.644708005294394));
#10672=CARTESIAN_POINT('Ctrl Pts',(12.60000518898,1.89417959722901,0.643846361750254));
#10673=CARTESIAN_POINT('Ctrl Pts',(12.6000052753339,1.8945988291305,0.642977876839351));
#10674=CARTESIAN_POINT('Ctrl Pts',(12.6000053405091,1.89500587920016,0.642102827114796));
#10675=CARTESIAN_POINT('Ctrl Pts',(12.6000058761205,1.89835102950234,0.634911640898031));
#10676=CARTESIAN_POINT('Ctrl Pts',(12.6000044960414,1.90083797337412,0.627363460372113));
#10677=CARTESIAN_POINT('Ctrl Pts',(12.6000025707297,1.90241244660326,0.619625605651968));
#10678=CARTESIAN_POINT('Ctrl Pts',(12.6000013488022,1.90341170938816,0.614714661398562));
#10679=CARTESIAN_POINT('Ctrl Pts',(12.5999999979477,1.90404256918024,0.609726685483646));
#10680=CARTESIAN_POINT('Ctrl Pts',(12.6000000000242,1.90428042250026,0.604702508168697));
#10681=CARTESIAN_POINT('',(12.6,-1.8038302225439,0.7));
#10682=CARTESIAN_POINT('',(12.6,-0.996884774049031,0.7));
#10683=CARTESIAN_POINT('Ctrl Pts',(12.6000000000242,-1.90428042250026,0.604702508168697));
#10684=CARTESIAN_POINT('Ctrl Pts',(12.5999999967566,-1.90390613686288,0.612608546261599));
#10685=CARTESIAN_POINT('Ctrl Pts',(12.6000030637542,-1.90256112855112,0.620429349781532));
#10686=CARTESIAN_POINT('Ctrl Pts',(12.6000044618611,-1.90032851942705,0.628004813168584));
#10687=CARTESIAN_POINT('Ctrl Pts',(12.6000051410147,-1.89924399238468,0.63168472059761));
#10688=CARTESIAN_POINT('Ctrl Pts',(12.6000055125137,-1.89794920179963,0.635306724151721));
#10689=CARTESIAN_POINT('Ctrl Pts',(12.6000054780251,-1.8964494555225,0.638851301608537));
#10690=CARTESIAN_POINT('Ctrl Pts',(12.6000054068101,-1.89335265044601,0.64617044994032));
#10691=CARTESIAN_POINT('Ctrl Pts',(12.6000033360581,-1.88942004582711,0.653077891556402));
#10692=CARTESIAN_POINT('Ctrl Pts',(12.6000021947065,-1.88472046879005,0.659412676045522));
#10693=CARTESIAN_POINT('Ctrl Pts',(12.6000018847951,-1.88344439178375,0.661132761228218));
#10694=CARTESIAN_POINT('Ctrl Pts',(12.6000016718208,-1.88211149822114,0.662810505670431));
#10695=CARTESIAN_POINT('Ctrl Pts',(12.6000016744967,-1.88072259784382,0.664442334323417));
#10696=CARTESIAN_POINT('Ctrl Pts',(12.6000016781594,-1.87882150924004,0.666675936463772));
#10697=CARTESIAN_POINT('Ctrl Pts',(12.6000020841502,-1.87681550570489,0.668823545630641));
#10698=CARTESIAN_POINT('Ctrl Pts',(12.6000026366798,-1.87471194035196,0.670881441794774));
#10699=CARTESIAN_POINT('Ctrl Pts',(12.6000041308351,-1.86902346102148,0.676446422116204));
#10700=CARTESIAN_POINT('Ctrl Pts',(12.600006461375,-1.86269053299793,0.681293522350018));
#10701=CARTESIAN_POINT('Ctrl Pts',(12.6000072160154,-1.85587841208407,0.685370830723365));
#10702=CARTESIAN_POINT('Ctrl Pts',(12.6000077023835,-1.85148797774957,0.687998669380522));
#10703=CARTESIAN_POINT('Ctrl Pts',(12.6000076405209,-1.84689749427555,0.690306084934615));
#10704=CARTESIAN_POINT('Ctrl Pts',(12.6000070464578,-1.84214500723865,0.692269637845719));
#10705=CARTESIAN_POINT('Ctrl Pts',(12.6000061272438,-1.8347913233911,0.69530790964196));
#10706=CARTESIAN_POINT('Ctrl Pts',(12.6000039197963,-1.82713360831075,0.697490862850871));
#10707=CARTESIAN_POINT('Ctrl Pts',(12.6000021173902,-1.81932000848244,0.698749700991972));
#10708=CARTESIAN_POINT('Ctrl Pts',(12.6000009388424,-1.81421089282246,0.699572823470905));
#10709=CARTESIAN_POINT('Ctrl Pts',(12.6,-1.80903450780073,0.7));
#10710=CARTESIAN_POINT('Ctrl Pts',(12.6,-1.80383022254432,0.7));
#10711=CARTESIAN_POINT('Ctrl Pts',(12.4277899437912,-1.91498765980368,8.1061082099175E-6));
#10712=CARTESIAN_POINT('Ctrl Pts',(12.4185093097394,-1.90440735427916,0.201956437811591));
#10713=CARTESIAN_POINT('Ctrl Pts',(12.4092288296506,-1.89382707230216,0.403904777849331));
#10714=CARTESIAN_POINT('Ctrl Pts',(12.3999485057213,-1.88324681432718,0.605853126346544));
#10715=CARTESIAN_POINT('Ctrl Pts',(11.2514531524596,-1.79377193015415,-0.000335869645892519));
#10716=CARTESIAN_POINT('Ctrl Pts',(11.2440495594319,-1.78319067664719,0.201611894978303));
#10717=CARTESIAN_POINT('Ctrl Pts',(11.2366461029568,-1.77260943823668,0.403559665746509));
#10718=CARTESIAN_POINT('Ctrl Pts',(11.2292427771396,-1.76202821861547,0.605507441576721));
#10719=CARTESIAN_POINT('Ctrl Pts',(10.0755218259154,-1.69940246002113,-0.00057195363688788));
#10720=CARTESIAN_POINT('Ctrl Pts',(10.0699958446785,-1.68882059084335,0.201375418496625));
#10721=CARTESIAN_POINT('Ctrl Pts',(10.0644699805481,-1.67823873210945,0.403322794723726));
#10722=CARTESIAN_POINT('Ctrl Pts',(10.0589442279885,-1.66765688783508,0.605270174140068));
#10723=CARTESIAN_POINT('Ctrl Pts',(8.90001330805802,-1.62424530699552,-0.000736768987564917));
#10724=CARTESIAN_POINT('Ctrl Pts',(8.89636559238287,-1.61366301035882,0.201210329036737));
#10725=CARTESIAN_POINT('Ctrl Pts',(8.89271797406169,-1.60308072296431,0.403157429313698));
#10726=CARTESIAN_POINT('Ctrl Pts',(8.88907045450167,-1.59249844499155,0.605104531878289));
#10727=CARTESIAN_POINT('Ctrl Pts',(8.9000000009702,-1.5932011715731,0.605106081469384));
#10728=CARTESIAN_POINT('Ctrl Pts',(10.0684994345535,-1.66840362346204,0.605023135335662));
#10729=CARTESIAN_POINT('Ctrl Pts',(11.2356615742313,-1.76272273105624,0.604904457271936));
#10730=CARTESIAN_POINT('Ctrl Pts',(12.4,-1.8833055216247,0.604732563714112));
#10731=CARTESIAN_POINT('Ctrl Pts',(12.8889963716306,-1.96391015057091,2.25514051876985E-16));
#10732=CARTESIAN_POINT('Ctrl Pts',(12.8789974396847,-1.95334878321431,0.201594505485581));
#10733=CARTESIAN_POINT('Ctrl Pts',(12.8689986695879,-1.94278744208821,0.403189020401051));
#10734=CARTESIAN_POINT('Ctrl Pts',(12.8590000636394,-1.93222612769726,0.604783544887274));
#10735=CARTESIAN_POINT('Ctrl Pts',(12.792662965057,-1.95339909479377,-3.05216148415599E-5));
#10736=CARTESIAN_POINT('Ctrl Pts',(12.7828174539371,-1.94283764251598,0.201563933758495));
#10737=CARTESIAN_POINT('Ctrl Pts',(12.7729721028852,-1.93227621586528,0.403158398317997));
#10738=CARTESIAN_POINT('Ctrl Pts',(12.7631269141758,-1.92171481533493,0.604752872200892));
#10739=CARTESIAN_POINT('Ctrl Pts',(12.6963322449993,-1.94307475200589,-6.02899321993968E-5));
#10740=CARTESIAN_POINT('Ctrl Pts',(12.6866401583647,-1.93251321719056,0.201534116532542));
#10741=CARTESIAN_POINT('Ctrl Pts',(12.6769482300299,-1.92195170741534,0.403128531945268));
#10742=CARTESIAN_POINT('Ctrl Pts',(12.6672564622455,-1.91139022316239,0.604722956439736));
#10743=CARTESIAN_POINT('Ctrl Pts',(12.6000042264769,-1.9329329264796,-8.93242901516475E-5));
#10744=CARTESIAN_POINT('Ctrl Pts',(12.5904655680581,-1.92237131142302,0.201505034443145));
#10745=CARTESIAN_POINT('Ctrl Pts',(12.5809270661843,-1.91180972083551,0.403099401891705));
#10746=CARTESIAN_POINT('Ctrl Pts',(12.5713887230828,-1.90124815518829,0.604693778185974));
#10747=CARTESIAN_POINT('',(12.8572578715866,-1.93204080633595,0.60466226999893));
#10748=CARTESIAN_POINT('Ctrl Pts',(12.6000000000242,-1.90428042250026,0.604702508168697));
#10749=CARTESIAN_POINT('Ctrl Pts',(12.6857696261193,-1.91338852735451,0.604689390578107));
#10750=CARTESIAN_POINT('Ctrl Pts',(12.7715225733429,-1.92264108900731,0.604675979983877));
#10751=CARTESIAN_POINT('Ctrl Pts',(12.8572578715866,-1.93204080633595,0.60466226999893));
#10752=CARTESIAN_POINT('Ctrl Pts',(12.8572578715866,-1.93204080633595,0.604662269998931));
#10753=CARTESIAN_POINT('Ctrl Pts',(12.867837444884,-1.94266422047353,0.403108198925376));
#10754=CARTESIAN_POINT('Ctrl Pts',(12.8784169445746,-1.95328733374019,0.201554108835025));
#10755=CARTESIAN_POINT('Ctrl Pts',(12.8889963716306,-1.96391015057091,-1.13624387676481E-16));
#10756=CARTESIAN_POINT('Ctrl Pts',(12.4102890066107,-1.7839488953552,0.7));
#10757=CARTESIAN_POINT('Ctrl Pts',(11.2423261062923,-1.6629989551888,0.7));
#10758=CARTESIAN_POINT('Ctrl Pts',(10.0717272052363,-1.56846077660453,0.7));
#10759=CARTESIAN_POINT('Ctrl Pts',(8.89999999999993,-1.49312521822106,0.7));
#10760=CARTESIAN_POINT('Ctrl Pts',(12.4072999778185,-1.81281269415102,0.7));
#10761=CARTESIAN_POINT('Ctrl Pts',(11.2397765858669,-1.69187462084457,0.699998757165067));
#10762=CARTESIAN_POINT('Ctrl Pts',(10.0695527221263,-1.59734372851255,0.700000594792869));
#10763=CARTESIAN_POINT('Ctrl Pts',(8.89814271406455,-1.52201240649035,0.7));
#10764=CARTESIAN_POINT('Ctrl Pts',(12.4021203845267,-1.86282985658401,0.676448561733929));
#10765=CARTESIAN_POINT('Ctrl Pts',(11.2353531757414,-1.74191593276004,0.676505236381959));
#10766=CARTESIAN_POINT('Ctrl Pts',(10.0657879841113,-1.64739716848489,0.676543604639643));
#10767=CARTESIAN_POINT('Ctrl Pts',(8.89492397206972,-1.57207492202614,0.676570833338327));
#10768=CARTESIAN_POINT('Ctrl Pts',(12.400106093269,-1.88228102337346,0.626471792264191));
#10769=CARTESIAN_POINT('Ctrl Pts',(11.2336287644773,-1.76143987438699,0.626617923584012));
#10770=CARTESIAN_POINT('Ctrl Pts',(10.0643137348541,-1.66697079985262,0.626717999675944));
#10771=CARTESIAN_POINT('Ctrl Pts',(8.89366330605793,-1.59168261717615,0.626788336025017));
#10772=CARTESIAN_POINT('Ctrl Pts',(12.4,-1.8833055216247,0.604732563714112));
#10773=CARTESIAN_POINT('Ctrl Pts',(11.2335332423564,-1.7625023138725,0.604904771481731));
#10774=CARTESIAN_POINT('Ctrl Pts',(10.0642324382527,-1.66805889332185,0.605023569028795));
#10775=CARTESIAN_POINT('Ctrl Pts',(8.89359217382714,-1.59278896817116,0.605106535971077));
#10776=CARTESIAN_POINT('Ctrl Pts',(12.400000003046,-1.78288409409898,0.7));
#10777=CARTESIAN_POINT('Ctrl Pts',(11.235451325406,-1.66244391065713,0.7));
#10778=CARTESIAN_POINT('Ctrl Pts',(10.0682865064676,-1.56823955876321,0.7));
#10779=CARTESIAN_POINT('Ctrl Pts',(8.89999999999993,-1.49312521822106,0.7));
#10780=CARTESIAN_POINT('Ctrl Pts',(12.8681436286308,-1.83274446434879,0.7));
#10781=CARTESIAN_POINT('Ctrl Pts',(12.7787800350189,-1.82294762441299,0.7));
#10782=CARTESIAN_POINT('Ctrl Pts',(12.6893984576578,-1.8133105623702,0.7));
#10783=CARTESIAN_POINT('Ctrl Pts',(12.6,-1.80383022254431,0.7));
#10784=CARTESIAN_POINT('Ctrl Pts',(12.8649798835675,-1.86160311979107,0.7));
#10785=CARTESIAN_POINT('Ctrl Pts',(12.7756511334299,-1.85180730951691,0.699999896874207));
#10786=CARTESIAN_POINT('Ctrl Pts',(12.686303642571,-1.84217134991284,0.700000098415946));
#10787=CARTESIAN_POINT('Ctrl Pts',(12.5969393303221,-1.83269196733649,0.7));
#10788=CARTESIAN_POINT('Ctrl Pts',(12.8594976525144,-1.91161025179704,0.676425356750174));
#10789=CARTESIAN_POINT('Ctrl Pts',(12.7702288461641,-1.90181652272411,0.676430055978541));
#10790=CARTESIAN_POINT('Ctrl Pts',(12.6809412203008,-1.89218243450198,0.676434576658958));
#10791=CARTESIAN_POINT('Ctrl Pts',(12.5916356538948,-1.88270499442535,0.67643906321291));
#10792=CARTESIAN_POINT('Ctrl Pts',(12.8573684983393,-1.93103170500986,0.626412260100396));
#10793=CARTESIAN_POINT('Ctrl Pts',(12.7681225846323,-1.92124403769089,0.626424372515079));
#10794=CARTESIAN_POINT('Ctrl Pts',(12.6788572782757,-1.91161594713487,0.626436135819418));
#10795=CARTESIAN_POINT('Ctrl Pts',(12.5895741974899,-1.90214427893475,0.626447702441804));
#10796=CARTESIAN_POINT('Ctrl Pts',(12.8572578715866,-1.93204080633595,0.60466226999893));
#10797=CARTESIAN_POINT('Ctrl Pts',(12.7680127446979,-1.92225628370762,0.604676541242762));
#10798=CARTESIAN_POINT('Ctrl Pts',(12.6787484942245,-1.91263121188365,0.60469048808123));
#10799=CARTESIAN_POINT('Ctrl Pts',(12.5894662143615,-1.9031625467727,0.604704117718382));
#10800=CARTESIAN_POINT('',(12.8681436286308,-1.83274446434879,0.7));
#10801=CARTESIAN_POINT('Ctrl Pts',(12.8681436286308,-1.83274446434879,0.7));
#10802=CARTESIAN_POINT('Ctrl Pts',(12.7787800350189,-1.82294762441299,0.7));
#10803=CARTESIAN_POINT('Ctrl Pts',(12.6893984576578,-1.8133105623702,0.7));
#10804=CARTESIAN_POINT('Ctrl Pts',(12.6,-1.80383022254431,0.7));
#10805=CARTESIAN_POINT('Origin',(12.8681436286308,-1.83274446434879,0.6));
#10806=CARTESIAN_POINT('Origin',(6.87409734069396,-2.22251806091942E-16,
0.7));
#10807=CARTESIAN_POINT('Ctrl Pts',(8.9,1.49312521822106,0.7));
#10808=CARTESIAN_POINT('Ctrl Pts',(10.0682865064677,1.56823955876321,0.7));
#10809=CARTESIAN_POINT('Ctrl Pts',(11.2354513254061,1.66244391065714,0.7));
#10810=CARTESIAN_POINT('Ctrl Pts',(12.4000000030461,1.78288409409899,0.7));
#10811=CARTESIAN_POINT('Origin',(6.87409734069396,-2.22251806091942E-16,
0.7));
#10812=CARTESIAN_POINT('',(12.8681436286308,1.83274446434879,0.7));
#10813=CARTESIAN_POINT('Ctrl Pts',(12.6,1.80383022254432,0.7));
#10814=CARTESIAN_POINT('Ctrl Pts',(12.6893984576578,1.8133105623702,0.7));
#10815=CARTESIAN_POINT('Ctrl Pts',(12.7787800350189,1.82294762441299,0.7));
#10816=CARTESIAN_POINT('Ctrl Pts',(12.8681436286308,1.83274446434879,0.7));
#10817=CARTESIAN_POINT('',(12.8681436286308,1.1,0.7));
#10818=CARTESIAN_POINT('Ctrl Pts',(8.9,1.49312521822106,0.7));
#10819=CARTESIAN_POINT('Ctrl Pts',(10.0717272052363,1.56846077660453,0.7));
#10820=CARTESIAN_POINT('Ctrl Pts',(11.2423261062923,1.6629989551888,0.7));
#10821=CARTESIAN_POINT('Ctrl Pts',(12.4102890066107,1.7839488953552,0.7));
#10822=CARTESIAN_POINT('Ctrl Pts',(8.89814271406461,1.52201240649035,0.7));
#10823=CARTESIAN_POINT('Ctrl Pts',(10.0695527221263,1.59734372851256,0.700000594792869));
#10824=CARTESIAN_POINT('Ctrl Pts',(11.2397765858669,1.69187462084457,0.699998757165067));
#10825=CARTESIAN_POINT('Ctrl Pts',(12.4072999778185,1.81281269415102,0.7));
#10826=CARTESIAN_POINT('Ctrl Pts',(8.89492397206979,1.57207492202615,0.676570833338327));
#10827=CARTESIAN_POINT('Ctrl Pts',(10.0657879841114,1.64739716848489,0.676543604639644));
#10828=CARTESIAN_POINT('Ctrl Pts',(11.2353531757414,1.74191593276004,0.676505236381959));
#10829=CARTESIAN_POINT('Ctrl Pts',(12.4021203845267,1.86282985658401,0.676448561733929));
#10830=CARTESIAN_POINT('Ctrl Pts',(8.89366330605799,1.59168261717616,0.626788336025017));
#10831=CARTESIAN_POINT('Ctrl Pts',(10.0643137348542,1.66697079985262,0.626717999675944));
#10832=CARTESIAN_POINT('Ctrl Pts',(11.2336287644773,1.761439874387,0.626617923584012));
#10833=CARTESIAN_POINT('Ctrl Pts',(12.400106093269,1.88228102337346,0.626471792264191));
#10834=CARTESIAN_POINT('Ctrl Pts',(8.89359217382721,1.59278896817116,0.605106535971077));
#10835=CARTESIAN_POINT('Ctrl Pts',(10.0642324382527,1.66805889332185,0.605023569028795));
#10836=CARTESIAN_POINT('Ctrl Pts',(11.2335332423565,1.7625023138725,0.604904771481731));
#10837=CARTESIAN_POINT('Ctrl Pts',(12.4,1.8833055216247,0.604732563714112));
#10838=CARTESIAN_POINT('Ctrl Pts',(12.4,1.8833055216247,0.604732563714112));
#10839=CARTESIAN_POINT('Ctrl Pts',(11.2356615742313,1.76272273105624,0.604904457271936));
#10840=CARTESIAN_POINT('Ctrl Pts',(10.0684994345535,1.66840362346204,0.605023135335662));
#10841=CARTESIAN_POINT('Ctrl Pts',(8.90000000097019,1.5932011715731,0.605106081469384));
#10842=CARTESIAN_POINT('Ctrl Pts',(8.90001330805765,1.62424530699444,-0.000736768966955875));
#10843=CARTESIAN_POINT('Ctrl Pts',(8.89636559238262,1.6136630103581,0.201210329050476));
#10844=CARTESIAN_POINT('Ctrl Pts',(8.89271797406156,1.60308072296395,0.403157429320568));
#10845=CARTESIAN_POINT('Ctrl Pts',(8.88907045450167,1.59249844499155,0.605104531878289));
#10846=CARTESIAN_POINT('Ctrl Pts',(10.0755218259151,1.69940246002007,-0.000571953616278766));
#10847=CARTESIAN_POINT('Ctrl Pts',(10.0699958446785,1.68882059084265,0.201375418510364));
#10848=CARTESIAN_POINT('Ctrl Pts',(10.0644699805483,1.67823873210911,0.403322794730596));
#10849=CARTESIAN_POINT('Ctrl Pts',(10.0589442279888,1.6676568878351,0.605270174140069));
#10850=CARTESIAN_POINT('Ctrl Pts',(11.2514531524595,1.79377193015312,-0.000335869625283423));
#10851=CARTESIAN_POINT('Ctrl Pts',(11.244049559432,1.78319067664652,0.201611894992042));
#10852=CARTESIAN_POINT('Ctrl Pts',(11.2366461029572,1.77260943823637,0.403559665753379));
#10853=CARTESIAN_POINT('Ctrl Pts',(11.2292427771402,1.76202821861552,0.605507441576721));
#10854=CARTESIAN_POINT('Ctrl Pts',(12.4277899437912,1.9149876598027,8.10612881915578E-6));
#10855=CARTESIAN_POINT('Ctrl Pts',(12.4185093097397,1.90440735427854,0.201956437825331));
#10856=CARTESIAN_POINT('Ctrl Pts',(12.4092288296513,1.89382707230189,0.403904777856201));
#10857=CARTESIAN_POINT('Ctrl Pts',(12.3999485057223,1.88324681432728,0.605853126346545));
#10858=CARTESIAN_POINT('Ctrl Pts',(12.6000042264759,1.9329329264795,-8.93242901520291E-5));
#10859=CARTESIAN_POINT('Ctrl Pts',(12.5904655680574,1.92237131142328,0.201505034436202));
#10860=CARTESIAN_POINT('Ctrl Pts',(12.580927066184,1.91180972083614,0.403099401877819));
#10861=CARTESIAN_POINT('Ctrl Pts',(12.5713887230828,1.90124815518927,0.604693778165146));
#10862=CARTESIAN_POINT('Ctrl Pts',(12.6963322449987,1.94307475200582,-6.02899321996874E-5));
#10863=CARTESIAN_POINT('Ctrl Pts',(12.6866401583644,1.93251321719085,0.201534116525599));
#10864=CARTESIAN_POINT('Ctrl Pts',(12.6769482300299,1.921951707416,0.403128531931383));
#10865=CARTESIAN_POINT('Ctrl Pts',(12.6672564622458,1.91139022316341,0.604722956418908));
#10866=CARTESIAN_POINT('Ctrl Pts',(12.7926629650567,1.95339909479374,-3.05216148420481E-5));
#10867=CARTESIAN_POINT('Ctrl Pts',(12.7828174539371,1.94283764251631,0.201563933751552));
#10868=CARTESIAN_POINT('Ctrl Pts',(12.7729721028855,1.93227621586597,0.403158398304112));
#10869=CARTESIAN_POINT('Ctrl Pts',(12.7631269141765,1.92171481533599,0.604752872180064));
#10870=CARTESIAN_POINT('Ctrl Pts',(12.8889963716306,1.96391015057091,-1.66533453693773E-16));
#10871=CARTESIAN_POINT('Ctrl Pts',(12.878997439685,1.95334878321468,0.201594505478638));
#10872=CARTESIAN_POINT('Ctrl Pts',(12.8689986695886,1.94278744208894,0.403189020387166));
#10873=CARTESIAN_POINT('Ctrl Pts',(12.8590000636404,1.93222612769835,0.604783544866446));
#10874=CARTESIAN_POINT('',(12.8572578715866,1.93204080633595,0.60466226999893));
#10875=CARTESIAN_POINT('Ctrl Pts',(12.8889963716306,1.96391015057091,-3.88144377749811E-17));
#10876=CARTESIAN_POINT('Ctrl Pts',(12.8784169445746,1.95328733374019,0.201554108835021));
#10877=CARTESIAN_POINT('Ctrl Pts',(12.867837444884,1.94266422047353,0.403108198925375));
#10878=CARTESIAN_POINT('Ctrl Pts',(12.8572578715866,1.93204080633595,0.604662269998929));
#10879=CARTESIAN_POINT('Ctrl Pts',(12.8572578715866,1.93204080633595,0.60466226999893));
#10880=CARTESIAN_POINT('Ctrl Pts',(12.7715225733429,1.92264108900731,0.604675979983877));
#10881=CARTESIAN_POINT('Ctrl Pts',(12.6857696261193,1.91338852735451,0.604689390578107));
#10882=CARTESIAN_POINT('Ctrl Pts',(12.6000000000242,1.90428042250026,0.604702508168697));
#10883=CARTESIAN_POINT('Origin',(8.7,1.68851851851852,0.));
#10884=CARTESIAN_POINT('',(8.7,-1.5805153611151,0.605119933308333));
#10885=CARTESIAN_POINT('Ctrl Pts',(8.7,-1.5805153611151,0.605119933308333));
#10886=CARTESIAN_POINT('Ctrl Pts',(8.7,-1.58569938832865,0.504197823486131));
#10887=CARTESIAN_POINT('Ctrl Pts',(8.7,-1.59088373519313,0.403275164205241));
#10888=CARTESIAN_POINT('Ctrl Pts',(8.7,-1.60124586355191,0.201568897935389));
#10889=CARTESIAN_POINT('Ctrl Pts',(8.7,-1.60642370224807,0.10078416210737));
#10890=CARTESIAN_POINT('Ctrl Pts',(8.7,-1.61160179736194,0.));
#10891=CARTESIAN_POINT('',(8.7,-1.48045180431786,0.7));
#10892=CARTESIAN_POINT('Ctrl Pts',(8.70000000036779,-1.48045180452391,0.7));
#10893=CARTESIAN_POINT('Ctrl Pts',(8.70000000202598,-1.48836706478042,0.699999999180279));
#10894=CARTESIAN_POINT('Ctrl Pts',(8.70000127066624,-1.49622113223642,0.699007614827928));
#10895=CARTESIAN_POINT('Ctrl Pts',(8.70000237141531,-1.50387364922569,0.697121884028934));
#10896=CARTESIAN_POINT('Ctrl Pts',(8.70000291188189,-1.50763102664002,0.696195992283305));
#10897=CARTESIAN_POINT('Ctrl Pts',(8.70000341240591,-1.51133980954515,0.695053883793301));
#10898=CARTESIAN_POINT('Ctrl Pts',(8.70000377175886,-1.51498230649063,0.693702880475192));
#10899=CARTESIAN_POINT('Ctrl Pts',(8.70000450976793,-1.52246296255016,0.690928302676144));
#10900=CARTESIAN_POINT('Ctrl Pts',(8.70000452394134,-1.52958344744078,0.687306123577328));
#10901=CARTESIAN_POINT('Ctrl Pts',(8.70000379461986,-1.53619834892264,0.682919715776694));
#10902=CARTESIAN_POINT('Ctrl Pts',(8.70000333219987,-1.54039247012311,0.680138551763745));
#10903=CARTESIAN_POINT('Ctrl Pts',(8.70000258238552,-1.54438316197938,0.67704909562189));
#10904=CARTESIAN_POINT('Ctrl Pts',(8.70000192913237,-1.54812716280968,0.67366362845569));
#10905=CARTESIAN_POINT('Ctrl Pts',(8.70000138361353,-1.55125370412533,0.670836491537814));
#10906=CARTESIAN_POINT('Ctrl Pts',(8.70000090341281,-1.55418891097064,0.66782012731024));
#10907=CARTESIAN_POINT('Ctrl Pts',(8.7000009033621,-1.55691103280728,0.664625500020687));
#10908=CARTESIAN_POINT('Ctrl Pts',(8.7000009032669,-1.56202159382457,0.658627848677152));
#10909=CARTESIAN_POINT('Ctrl Pts',(8.70000241148087,-1.56638404855443,0.652003279246098));
#10910=CARTESIAN_POINT('Ctrl Pts',(8.70000292788623,-1.5699383402149,0.64491699469699));
#10911=CARTESIAN_POINT('Ctrl Pts',(8.70000298354275,-1.57032141040405,0.644153257609021));
#10912=CARTESIAN_POINT('Ctrl Pts',(8.70000303046442,-1.57069504840788,0.643384135640712));
#10913=CARTESIAN_POINT('Ctrl Pts',(8.70000306761332,-1.57105914547653,0.642609822781892));
#10914=CARTESIAN_POINT('Ctrl Pts',(8.70000341208914,-1.57443535963509,0.635429742901602));
#10915=CARTESIAN_POINT('Ctrl Pts',(8.70000263566904,-1.57695592401075,0.627888404173009));
#10916=CARTESIAN_POINT('Ctrl Pts',(8.70000151703179,-1.57856725066757,0.620153930269154));
#10917=CARTESIAN_POINT('Ctrl Pts',(8.70000080174396,-1.57959757782623,0.615208292159515));
#10918=CARTESIAN_POINT('Ctrl Pts',(8.7,-1.58025528705454,0.610183028431161));
#10919=CARTESIAN_POINT('Ctrl Pts',(8.7,-1.5805153611151,0.605119933308333));
#10920=CARTESIAN_POINT('',(8.7,1.48045180431904,0.7));
#10921=CARTESIAN_POINT('',(8.7,0.844259259259259,0.7));
#10922=CARTESIAN_POINT('',(8.7,1.5805153611151,0.605119933308333));
#10923=CARTESIAN_POINT('Ctrl Pts',(8.7,1.5805153611151,0.605119933308333));
#10924=CARTESIAN_POINT('Ctrl Pts',(8.7,1.58010890623597,0.61303275518587));
#10925=CARTESIAN_POINT('Ctrl Pts',(8.70000179355525,1.57873376841273,0.620855553142259));
#10926=CARTESIAN_POINT('Ctrl Pts',(8.7000025961206,1.5764741717406,0.62842799710221));
#10927=CARTESIAN_POINT('Ctrl Pts',(8.70000304562639,1.57520860278123,0.632669218617747));
#10928=CARTESIAN_POINT('Ctrl Pts',(8.70000324668712,1.57366457852079,0.636831947144834));
#10929=CARTESIAN_POINT('Ctrl Pts',(8.70000313318341,1.57185009366145,0.640886032861668));
#10930=CARTESIAN_POINT('Ctrl Pts',(8.70000293045856,1.56860930815545,0.648126888117959));
#10931=CARTESIAN_POINT('Ctrl Pts',(8.70000158438082,1.56454425420738,0.654942317779106));
#10932=CARTESIAN_POINT('Ctrl Pts',(8.70000106269264,1.55971945710293,0.661169479919421));
#10933=CARTESIAN_POINT('Ctrl Pts',(8.70000096439252,1.55881033523018,0.662342845179011));
#10934=CARTESIAN_POINT('Ctrl Pts',(8.70000090351839,1.55787410801649,0.663495254390581));
#10935=CARTESIAN_POINT('Ctrl Pts',(8.70000090409683,1.55691103285321,0.664625500020665));
#10936=CARTESIAN_POINT('Ctrl Pts',(8.70000090523835,1.55501044337284,0.666855993586132));
#10937=CARTESIAN_POINT('Ctrl Pts',(8.70000114361209,1.55300532702719,0.669000219206223));
#10938=CARTESIAN_POINT('Ctrl Pts',(8.70000146777886,1.55090303951829,0.671054438207787));
#10939=CARTESIAN_POINT('Ctrl Pts',(8.70000234447876,1.54521746205001,0.676610015749294));
#10940=CARTESIAN_POINT('Ctrl Pts',(8.70000370702799,1.53888821826629,0.681447385411957));
#10941=CARTESIAN_POINT('Ctrl Pts',(8.70000415375638,1.53207947242364,0.685512859850771));
#10942=CARTESIAN_POINT('Ctrl Pts',(8.70000443876751,1.52773551673798,0.688106618115728));
#10943=CARTESIAN_POINT('Ctrl Pts',(8.70000441165582,1.52319541573235,0.690385508075002));
#10944=CARTESIAN_POINT('Ctrl Pts',(8.70000407315693,1.51849599021366,0.692326230693156));
#10945=CARTESIAN_POINT('Ctrl Pts',(8.70000354533424,1.51116815716702,0.695352407250086));
#10946=CARTESIAN_POINT('Ctrl Pts',(8.70000225790696,1.50353761203248,0.697524030080351));
#10947=CARTESIAN_POINT('Ctrl Pts',(8.70000121423997,1.49575164755759,0.698771658000832));
#10948=CARTESIAN_POINT('Ctrl Pts',(8.70000053774506,1.49070486028667,0.699580358416591));
#10949=CARTESIAN_POINT('Ctrl Pts',(8.70000000144466,1.48559217323052,0.699999999467653));
#10950=CARTESIAN_POINT('Ctrl Pts',(8.70000000036779,1.48045180452391,0.7));
#10951=CARTESIAN_POINT('Ctrl Pts',(8.7,1.61160179736194,0.));
#10952=CARTESIAN_POINT('Ctrl Pts',(8.7,1.60642368739695,0.100784451162898));
#10953=CARTESIAN_POINT('Ctrl Pts',(8.7,1.60124583384883,0.201569476094892));
#10954=CARTESIAN_POINT('Ctrl Pts',(8.7,1.59088370548997,0.403275742430776));
#10955=CARTESIAN_POINT('Ctrl Pts',(8.7,1.58569937347746,0.504198112607714));
#10956=CARTESIAN_POINT('Ctrl Pts',(8.7,1.5805153611151,0.605119933308333));
#10957=CARTESIAN_POINT('Ctrl Pts',(8.7100201910492,-1.61222456240079,1.33887903992595E-6));
#10958=CARTESIAN_POINT('Ctrl Pts',(8.70667727354472,-1.60164608969543,0.201874135619687));
#10959=CARTESIAN_POINT('Ctrl Pts',(8.70333445073708,-1.59106762573893,0.40374693439627));
#10960=CARTESIAN_POINT('Ctrl Pts',(8.69999172399519,-1.58048917070122,0.605619735240497));
#10961=CARTESIAN_POINT('Ctrl Pts',(7.30266630830786,-1.52469223633113,-0.000186944012493601));
#10962=CARTESIAN_POINT('Ctrl Pts',(7.3015714609838,-1.51411327886182,0.201685539385837));
#10963=CARTESIAN_POINT('Ctrl Pts',(7.30047669312962,-1.50353432123569,0.403558023359813));
#10964=CARTESIAN_POINT('Ctrl Pts',(7.2993819983171,-1.49295537435081,0.605430507723141));
#10965=CARTESIAN_POINT('Ctrl Pts',(5.89591889571946,-1.46411055243784,-0.000276130330627546));
#10966=CARTESIAN_POINT('Ctrl Pts',(5.8970730573458,-1.45353136553189,0.201596203763285));
#10967=CARTESIAN_POINT('Ctrl Pts',(5.89822728315403,-1.44295217665945,0.403468537584815));
#10968=CARTESIAN_POINT('Ctrl Pts',(5.89938156763751,-1.43237299696387,0.60534087113472));
#10969=CARTESIAN_POINT('Ctrl Pts',(4.48978738186403,-1.41740792524342,-0.000330195618103912));
#10970=CARTESIAN_POINT('Ctrl Pts',(4.49319153668887,-1.4068286019831,0.201542048187911));
#10971=CARTESIAN_POINT('Ctrl Pts',(4.49659574248722,-1.39624928130228,0.403414291272231));
#10972=CARTESIAN_POINT('Ctrl Pts',(4.5,-1.3856699632509,0.605286533625018));
#10973=CARTESIAN_POINT('Ctrl Pts',(4.50000000014037,-1.38566996330298,0.605286533623957));
#10974=CARTESIAN_POINT('Ctrl Pts',(5.90109530155974,-1.43243455365708,0.605259331490037));
#10975=CARTESIAN_POINT('Ctrl Pts',(7.30150776148394,-1.49309969195427,0.605214402664297));
#10976=CARTESIAN_POINT('Ctrl Pts',(8.7,-1.5805153611151,0.605119933308333));
#10977=CARTESIAN_POINT('Ctrl Pts',(8.7062300060629,-1.48084102486261,0.7));
#10978=CARTESIAN_POINT('Ctrl Pts',(7.30535837857749,-1.39328148786737,0.7));
#10979=CARTESIAN_POINT('Ctrl Pts',(5.90286553803659,-1.3325543763676,0.7));
#10980=CARTESIAN_POINT('Ctrl Pts',(4.5,-1.28575421950843,0.7));
#10981=CARTESIAN_POINT('Ctrl Pts',(8.7044244076592,-1.50972892972339,0.7));
#10982=CARTESIAN_POINT('Ctrl Pts',(7.30392377861185,-1.42217417124324,0.699999322371676));
#10983=CARTESIAN_POINT('Ctrl Pts',(5.90170976758769,-1.36144968116949,0.700000194339816));
#10984=CARTESIAN_POINT('Ctrl Pts',(4.49903600403804,-1.314650633636,0.7));
#10985=CARTESIAN_POINT('Ctrl Pts',(8.70129509098077,-1.55979510296572,0.676577193851887));
#10986=CARTESIAN_POINT('Ctrl Pts',(7.30143307762773,-1.47225060169427,0.676608218952397));
#10987=CARTESIAN_POINT('Ctrl Pts',(5.89970879741633,-1.41153023905743,0.676622651488038));
#10988=CARTESIAN_POINT('Ctrl Pts',(4.49736521340071,-1.36473368385825,0.676631564755462));
#10989=CARTESIAN_POINT('Ctrl Pts',(8.70006933407556,-1.57940608001781,0.626799670546273));
#10990=CARTESIAN_POINT('Ctrl Pts',(7.3004573192207,-1.49190036240803,0.626879818917698));
#10991=CARTESIAN_POINT('Ctrl Pts',(5.89892183391985,-1.43119871194172,0.62691759730524));
#10992=CARTESIAN_POINT('Ctrl Pts',(4.49670869913724,-1.38441313147668,0.626940642142451));
#10993=CARTESIAN_POINT('Ctrl Pts',(8.7,-1.5805153611151,0.605119933308333));
#10994=CARTESIAN_POINT('Ctrl Pts',(7.30039998287682,-1.49303044794594,0.605214477495697));
#10995=CARTESIAN_POINT('Ctrl Pts',(5.89887670103551,-1.4323384618751,0.605259402637312));
#10996=CARTESIAN_POINT('Ctrl Pts',(4.49667047719213,-1.38555885946567,0.605286598232956));
#10997=CARTESIAN_POINT('Ctrl Pts',(8.70000000036771,-1.48045180452391,0.7));
#10998=CARTESIAN_POINT('Ctrl Pts',(7.30120024114866,-1.39310147361351,0.7));
#10999=CARTESIAN_POINT('Ctrl Pts',(5.90078591724148,-1.332484999384,0.7));
#11000=CARTESIAN_POINT('Ctrl Pts',(4.5,-1.28575421950843,0.7));
#11001=CARTESIAN_POINT('Origin',(6.87409734069396,-2.22251806091942E-16,
0.7));
#11002=CARTESIAN_POINT('Ctrl Pts',(4.5,1.28575421950843,0.7));
#11003=CARTESIAN_POINT('Ctrl Pts',(5.9007859172415,1.332484999384,0.7));
#11004=CARTESIAN_POINT('Ctrl Pts',(7.30120024114871,1.39310147361351,0.7));
#11005=CARTESIAN_POINT('Ctrl Pts',(8.70000000036779,1.48045180452391,0.7));
#11006=CARTESIAN_POINT('Ctrl Pts',(4.5,1.28575421950843,0.7));
#11007=CARTESIAN_POINT('Ctrl Pts',(5.90286553803659,1.3325543763676,0.7));
#11008=CARTESIAN_POINT('Ctrl Pts',(7.30535837857749,1.39328148786737,0.7));
#11009=CARTESIAN_POINT('Ctrl Pts',(8.7062300060629,1.48084102486261,0.7));
#11010=CARTESIAN_POINT('Ctrl Pts',(4.49903600403804,1.314650633636,0.7));
#11011=CARTESIAN_POINT('Ctrl Pts',(5.90170976758769,1.36144968116949,0.700000194339816));
#11012=CARTESIAN_POINT('Ctrl Pts',(7.30392377861185,1.42217417124324,0.699999322371676));
#11013=CARTESIAN_POINT('Ctrl Pts',(8.7044244076592,1.50972892972339,0.7));
#11014=CARTESIAN_POINT('Ctrl Pts',(4.49736521340071,1.36473368385825,0.676631564755462));
#11015=CARTESIAN_POINT('Ctrl Pts',(5.89970879741633,1.41153023905743,0.676622651488038));
#11016=CARTESIAN_POINT('Ctrl Pts',(7.30143307762774,1.47225060169427,0.676608218952397));
#11017=CARTESIAN_POINT('Ctrl Pts',(8.70129509098078,1.55979510296572,0.676577193851887));
#11018=CARTESIAN_POINT('Ctrl Pts',(4.49670869913724,1.38441313147668,0.626940642142451));
#11019=CARTESIAN_POINT('Ctrl Pts',(5.89892183391985,1.43119871194172,0.626917597305239));
#11020=CARTESIAN_POINT('Ctrl Pts',(7.3004573192207,1.49190036240803,0.626879818917698));
#11021=CARTESIAN_POINT('Ctrl Pts',(8.70006933407556,1.57940608001781,0.626799670546273));
#11022=CARTESIAN_POINT('Ctrl Pts',(4.49667047719213,1.38555885946567,0.605286598232956));
#11023=CARTESIAN_POINT('Ctrl Pts',(5.89887670103551,1.4323384618751,0.605259402637312));
#11024=CARTESIAN_POINT('Ctrl Pts',(7.30039998287682,1.49303044794594,0.605214477495697));
#11025=CARTESIAN_POINT('Ctrl Pts',(8.7,1.5805153611151,0.605119933308333));
#11026=CARTESIAN_POINT('Ctrl Pts',(8.7,1.5805153611151,0.605119933308333));
#11027=CARTESIAN_POINT('Ctrl Pts',(7.30150776148394,1.49309969195427,0.605214402664297));
#11028=CARTESIAN_POINT('Ctrl Pts',(5.90109530155974,1.43243455365708,0.605259331490037));
#11029=CARTESIAN_POINT('Ctrl Pts',(4.50000000014037,1.38566996330298,0.605286533623957));
#11030=CARTESIAN_POINT('Ctrl Pts',(4.48978738186405,1.41740792524342,-0.00033019561810394));
#11031=CARTESIAN_POINT('Ctrl Pts',(4.49319153668889,1.40682860198312,0.201542048187577));
#11032=CARTESIAN_POINT('Ctrl Pts',(4.49659574248723,1.39624928130232,0.403414291271564));
#11033=CARTESIAN_POINT('Ctrl Pts',(4.5,1.38566996325095,0.605286533624017));
#11034=CARTESIAN_POINT('Ctrl Pts',(5.89591889571947,1.46411055243784,-0.000276130330627574));
#11035=CARTESIAN_POINT('Ctrl Pts',(5.89707305734581,1.45353136553191,0.201596203762952));
#11036=CARTESIAN_POINT('Ctrl Pts',(5.89822728315404,1.44295217665948,0.403468537584147));
#11037=CARTESIAN_POINT('Ctrl Pts',(5.89938156763751,1.43237299696393,0.605340871133719));
#11038=CARTESIAN_POINT('Ctrl Pts',(7.30266630830786,1.52469223633113,-0.000186944012493549));
#11039=CARTESIAN_POINT('Ctrl Pts',(7.3015714609838,1.51411327886184,0.201685539385503));
#11040=CARTESIAN_POINT('Ctrl Pts',(7.30047669312963,1.50353432123572,0.403558023359145));
#11041=CARTESIAN_POINT('Ctrl Pts',(7.29938199831711,1.49295537435086,0.60543050772214));
#11042=CARTESIAN_POINT('Ctrl Pts',(8.7100201910492,1.61222456240079,1.33887903989646E-6));
#11043=CARTESIAN_POINT('Ctrl Pts',(8.70667727354472,1.60164608969545,0.201874135619353));
#11044=CARTESIAN_POINT('Ctrl Pts',(8.7033344507371,1.59106762573896,0.403746934395602));
#11045=CARTESIAN_POINT('Ctrl Pts',(8.6999917239952,1.58048917070127,0.605619735239495));
#11046=CARTESIAN_POINT('Origin',(4.3,1.48481481481482,0.));
#11047=CARTESIAN_POINT('',(4.3,-1.37908752581626,0.605290299758539));
#11048=CARTESIAN_POINT('Ctrl Pts',(4.3,-1.37908752581626,0.605290299758539));
#11049=CARTESIAN_POINT('Ctrl Pts',(4.3,-1.38444464017247,0.504222347694443));
#11050=CARTESIAN_POINT('Ctrl Pts',(4.3,-1.38980163214303,0.403154389143214));
#11051=CARTESIAN_POINT('Ctrl Pts',(4.3,-1.40049562949383,0.201390955816302));
#11052=CARTESIAN_POINT('Ctrl Pts',(4.3,-1.40583263576898,0.100695481088992));
#11053=CARTESIAN_POINT('Ctrl Pts',(4.3,-1.41116952203211,0.));
#11054=CARTESIAN_POINT('Ctrl Pts',(4.30000000005992,-1.27917501058303,0.7));
#11055=CARTESIAN_POINT('Ctrl Pts',(4.30000000048661,-1.28708628524264,0.699999999884766));
#11056=CARTESIAN_POINT('Ctrl Pts',(4.30000064978116,-1.29493415608545,0.69900616264686));
#11057=CARTESIAN_POINT('Ctrl Pts',(4.30000121018478,-1.30257825621016,0.697119208693397));
#11058=CARTESIAN_POINT('Ctrl Pts',(4.30000152558655,-1.30688044586137,0.696057208766858));
#11059=CARTESIAN_POINT('Ctrl Pts',(4.30000181105247,-1.31111814675806,0.694711271736901));
#11060=CARTESIAN_POINT('Ctrl Pts',(4.30000199036827,-1.31526464671957,0.693092387263961));
#11061=CARTESIAN_POINT('Ctrl Pts',(4.30000231141323,-1.32268849323592,0.690193954859197));
#11062=CARTESIAN_POINT('Ctrl Pts',(4.30000222777046,-1.32973966400828,0.686455190804221));
#11063=CARTESIAN_POINT('Ctrl Pts',(4.30000179417102,-1.33627196700415,0.681957645816867));
#11064=CARTESIAN_POINT('Ctrl Pts',(4.30000155535849,-1.33986974800182,0.679480543652151));
#11065=CARTESIAN_POINT('Ctrl Pts',(4.30000121902461,-1.34330986828215,0.67677238407294));
#11066=CARTESIAN_POINT('Ctrl Pts',(4.30000092191081,-1.34656397897095,0.673841242448196));
#11067=CARTESIAN_POINT('Ctrl Pts',(4.30000063243573,-1.34973442737118,0.670985459666446));
#11068=CARTESIAN_POINT('Ctrl Pts',(4.30000037658882,-1.35270906921767,0.667935271966333));
#11069=CARTESIAN_POINT('Ctrl Pts',(4.30000037869864,-1.35546536049262,0.66470214425512));
#11070=CARTESIAN_POINT('Ctrl Pts',(4.30000038260995,-1.36057515211559,0.658708362304413));
#11071=CARTESIAN_POINT('Ctrl Pts',(4.30000117797282,-1.36493744806469,0.652087250959406));
#11072=CARTESIAN_POINT('Ctrl Pts',(4.30000145944905,-1.36849285270534,0.645004510397983));
#11073=CARTESIAN_POINT('Ctrl Pts',(4.30000148826005,-1.36885677248754,0.644279543857467));
#11074=CARTESIAN_POINT('Ctrl Pts',(4.30000151299237,-1.36921219826683,0.643549721050429));
#11075=CARTESIAN_POINT('Ctrl Pts',(4.30000153317099,-1.36955903781249,0.642815208524159));
#11076=CARTESIAN_POINT('Ctrl Pts',(4.30000173031152,-1.37294758118467,0.635639188419686));
#11077=CARTESIAN_POINT('Ctrl Pts',(4.30000134819424,-1.37548140076902,0.628100134775109));
#11078=CARTESIAN_POINT('Ctrl Pts',(4.30000077902196,-1.37710733725971,0.620366659714886));
#11079=CARTESIAN_POINT('Ctrl Pts',(4.30000041405338,-1.37814993145247,0.615407747584041));
#11080=CARTESIAN_POINT('Ctrl Pts',(4.3,-1.37881837002099,0.610368224776708));
#11081=CARTESIAN_POINT('Ctrl Pts',(4.3,-1.37908752581626,0.605290299758539));
#11082=CARTESIAN_POINT('',(4.3,1.37908752581626,0.605290299758539));
#11083=CARTESIAN_POINT('Ctrl Pts',(4.3,1.37908752581626,0.605290299758539));
#11084=CARTESIAN_POINT('Ctrl Pts',(4.3,1.37866806817032,0.613203837240499));
#11085=CARTESIAN_POINT('Ctrl Pts',(4.30000092021544,1.37728139671899,0.621026590428679));
#11086=CARTESIAN_POINT('Ctrl Pts',(4.30000132151137,1.37501133257008,0.628597948954885));
#11087=CARTESIAN_POINT('Ctrl Pts',(4.30000154544343,1.37374458621782,0.632822935636113));
#11088=CARTESIAN_POINT('Ctrl Pts',(4.30000164013187,1.37220176226583,0.636969676056352));
#11089=CARTESIAN_POINT('Ctrl Pts',(4.30000157305315,1.37039070587839,0.641008268098125));
#11090=CARTESIAN_POINT('Ctrl Pts',(4.30000145288191,1.36714620633991,0.648243387946652));
#11091=CARTESIAN_POINT('Ctrl Pts',(4.30000073948134,1.36307905360626,0.655053358422861));
#11092=CARTESIAN_POINT('Ctrl Pts',(4.3000004635866,1.35825284513469,0.661274801567968));
#11093=CARTESIAN_POINT('Ctrl Pts',(4.30000041199046,1.35735027731582,0.662438297592388));
#11094=CARTESIAN_POINT('Ctrl Pts',(4.30000037986005,1.35642103364291,0.663581140343808));
#11095=CARTESIAN_POINT('Ctrl Pts',(4.30000037943224,1.35546536051643,0.664702144255114));
#11096=CARTESIAN_POINT('Ctrl Pts',(4.300000378582,1.3535659898678,0.666930104702213));
#11097=CARTESIAN_POINT('Ctrl Pts',(4.3000005018795,1.35156225525783,0.669071850305581));
#11098=CARTESIAN_POINT('Ctrl Pts',(4.30000067038034,1.34946148384904,0.671123623013939));
#11099=CARTESIAN_POINT('Ctrl Pts',(4.30000112630012,1.34377733881547,0.676675190215126));
#11100=CARTESIAN_POINT('Ctrl Pts',(4.30000183907902,1.33744971106208,0.68150833207295));
#11101=CARTESIAN_POINT('Ctrl Pts',(4.30000208123143,1.33064243458576,0.685568782013219));
#11102=CARTESIAN_POINT('Ctrl Pts',(4.30000223513396,1.3263159977886,0.688149444058562));
#11103=CARTESIAN_POINT('Ctrl Pts',(4.3000022300233,1.32179485563522,0.690417305529342));
#11104=CARTESIAN_POINT('Ctrl Pts',(4.30000206344016,1.31711540146937,0.692349146556373));
#11105=CARTESIAN_POINT('Ctrl Pts',(4.3000018029167,1.30979708846622,0.695370400063095));
#11106=CARTESIAN_POINT('Ctrl Pts',(4.30000114702936,1.30217656646843,0.69753735975804));
#11107=CARTESIAN_POINT('Ctrl Pts',(4.3000006156201,1.29440092269557,0.69878042986007));
#11108=CARTESIAN_POINT('Ctrl Pts',(4.30000027236218,1.28937833178082,0.699583377215073));
#11109=CARTESIAN_POINT('Ctrl Pts',(4.30000000033581,1.28429042584107,0.69999999992549));
#11110=CARTESIAN_POINT('Ctrl Pts',(4.30000000005992,1.27917501058303,0.7));
#11111=CARTESIAN_POINT('Ctrl Pts',(4.3,1.41116952203211,0.));
#11112=CARTESIAN_POINT('Ctrl Pts',(4.3,1.40583262613343,0.100695662891028));
#11113=CARTESIAN_POINT('Ctrl Pts',(4.3,1.40049561022223,0.201391319421434));
#11114=CARTESIAN_POINT('Ctrl Pts',(4.3,1.38980161287056,0.403154752748307));
#11115=CARTESIAN_POINT('Ctrl Pts',(4.3,1.38444463053604,0.504222529496425));
#11116=CARTESIAN_POINT('Ctrl Pts',(4.3,1.37908752581626,0.605290299758539));
#11117=CARTESIAN_POINT('Ctrl Pts',(4.3,-1.41116952203217,-1.08233907947231E-12));
#11118=CARTESIAN_POINT('Ctrl Pts',(4.30370667985561,-1.40059355144761,0.201807922462111));
#11119=CARTESIAN_POINT('Ctrl Pts',(4.30741340932898,-1.39001758331341,0.403615844144917));
#11120=CARTESIAN_POINT('Ctrl Pts',(4.31112018914117,-1.37944161767694,0.605423765036612));
#11121=CARTESIAN_POINT('Ctrl Pts',(3.22410085073145,-1.37636920007795,-3.90459529712038E-5));
#11122=CARTESIAN_POINT('Ctrl Pts',(3.2295286994181,-1.36579313421488,0.201768811380596));
#11123=CARTESIAN_POINT('Ctrl Pts',(3.23495659078338,-1.35521706809947,0.403576667516588));
#11124=CARTESIAN_POINT('Ctrl Pts',(3.24038452463065,-1.34464100578453,0.605384522622892));
#11125=CARTESIAN_POINT('Ctrl Pts',(2.14856196511704,-1.34935185539723,-5.92140864038068E-5));
#11126=CARTESIAN_POINT('Ctrl Pts',(2.15571155670467,-1.33877574824886,0.201748609775608));
#11127=CARTESIAN_POINT('Ctrl Pts',(2.16286118630165,-1.32819964054015,0.403556432267456));
#11128=CARTESIAN_POINT('Ctrl Pts',(2.17001085376486,-1.31762353633116,0.605364253566666));
#11129=CARTESIAN_POINT('Ctrl Pts',(1.073384157387,-1.32427529283232,-8.86713468529234E-5));
#11130=CARTESIAN_POINT('Ctrl Pts',(1.08225606990756,-1.31369916974321,0.201719104822629));
#11131=CARTESIAN_POINT('Ctrl Pts',(1.09112801825726,-1.30312304798914,0.403526879488275));
#11132=CARTESIAN_POINT('Ctrl Pts',(1.10000000295732,-1.29254692759565,0.605334652628532));
#11133=CARTESIAN_POINT('Ctrl Pts',(1.10000000298281,-1.29254692760111,0.605334652628557));
#11134=CARTESIAN_POINT('Ctrl Pts',(2.16694388170712,-1.31755402957363,0.605319894542965));
#11135=CARTESIAN_POINT('Ctrl Pts',(3.23367147240841,-1.34448060345116,0.605309774863278));
#11136=CARTESIAN_POINT('Ctrl Pts',(4.3,-1.37908752581626,0.605290299758539));
#11137=CARTESIAN_POINT('Ctrl Pts',(4.30323908112369,-1.2792801058419,0.7));
#11138=CARTESIAN_POINT('Ctrl Pts',(3.23565147654712,-1.24463335454069,0.7));
#11139=CARTESIAN_POINT('Ctrl Pts',(2.1678436779024,-1.21768649131741,0.7));
#11140=CARTESIAN_POINT('Ctrl Pts',(1.09999999999999,-1.19266190204553,0.7));
#11141=CARTESIAN_POINT('Ctrl Pts',(4.30230129178181,-1.30817667592415,0.7));
#11142=CARTESIAN_POINT('Ctrl Pts',(3.23485320804887,-1.27353066282864,0.699999860738333));
#11143=CARTESIAN_POINT('Ctrl Pts',(2.16713169816659,-1.24658393122273,0.700000105496227));
#11144=CARTESIAN_POINT('Ctrl Pts',(1.0993228455422,-1.22155728565617,0.7));
#11145=CARTESIAN_POINT('Ctrl Pts',(4.30067574076257,-1.35826558912881,0.676637683834297));
#11146=CARTESIAN_POINT('Ctrl Pts',(3.23346787205668,-1.32362126434549,0.676644071225102));
#11147=CARTESIAN_POINT('Ctrl Pts',(2.16589795861771,-1.29667457247055,0.676647306834711));
#11148=CARTESIAN_POINT('Ctrl Pts',(1.09814906228501,-1.27164470234869,0.676652147774997));
#11149=CARTESIAN_POINT('Ctrl Pts',(4.30003720890047,-1.37794098943329,0.626943772371838));
#11150=CARTESIAN_POINT('Ctrl Pts',(3.23292426239396,-1.34330449078822,0.626960286972675));
#11151=CARTESIAN_POINT('Ctrl Pts',(2.16541285690349,-1.31636171257899,0.6269687859393));
#11152=CARTESIAN_POINT('Ctrl Pts',(1.09768760301306,-1.29133598921902,0.626981304916489));
#11153=CARTESIAN_POINT('Ctrl Pts',(4.3,-1.37908752581626,0.605290299758539));
#11154=CARTESIAN_POINT('Ctrl Pts',(3.23289209128077,-1.34445530919946,0.605309789097661));
#11155=CARTESIAN_POINT('Ctrl Pts',(2.16538453588699,-1.31751467232976,0.605319909330946));
#11156=CARTESIAN_POINT('Ctrl Pts',(1.09766050997011,-1.29249209748956,0.605334684996117));
#11157=CARTESIAN_POINT('Ctrl Pts',(1.09999999999999,1.19266190204553,0.7));
#11158=CARTESIAN_POINT('Ctrl Pts',(2.1678436779024,1.21768649131741,0.7));
#11159=CARTESIAN_POINT('Ctrl Pts',(3.23565147654712,1.24463335454069,0.7));
#11160=CARTESIAN_POINT('Ctrl Pts',(4.30323908112369,1.2792801058419,0.7));
#11161=CARTESIAN_POINT('Ctrl Pts',(1.0993228455422,1.22155728565617,0.7));
#11162=CARTESIAN_POINT('Ctrl Pts',(2.16713169816659,1.24658393122273,0.700000105496227));
#11163=CARTESIAN_POINT('Ctrl Pts',(3.23485320804887,1.27353066282864,0.699999860738333));
#11164=CARTESIAN_POINT('Ctrl Pts',(4.30230129178181,1.30817667592415,0.7));
#11165=CARTESIAN_POINT('Ctrl Pts',(1.09814906228501,1.27164470234869,0.676652147774997));
#11166=CARTESIAN_POINT('Ctrl Pts',(2.16589795861771,1.29667457247055,0.676647306834711));
#11167=CARTESIAN_POINT('Ctrl Pts',(3.23346787205668,1.32362126434549,0.676644071225102));
#11168=CARTESIAN_POINT('Ctrl Pts',(4.30067574076257,1.35826558912881,0.676637683834297));
#11169=CARTESIAN_POINT('Ctrl Pts',(1.09768760301306,1.29133598921902,0.626981304916489));
#11170=CARTESIAN_POINT('Ctrl Pts',(2.16541285690349,1.31636171257899,0.6269687859393));
#11171=CARTESIAN_POINT('Ctrl Pts',(3.23292426239396,1.34330449078822,0.626960286972675));
#11172=CARTESIAN_POINT('Ctrl Pts',(4.30003720890047,1.37794098943329,0.626943772371838));
#11173=CARTESIAN_POINT('Ctrl Pts',(1.09766050997011,1.29249209748956,0.605334684996117));
#11174=CARTESIAN_POINT('Ctrl Pts',(2.16538453588699,1.31751467232976,0.605319909330946));
#11175=CARTESIAN_POINT('Ctrl Pts',(3.23289209128077,1.34445530919946,0.605309789097661));
#11176=CARTESIAN_POINT('Ctrl Pts',(4.3,1.37908752581626,0.605290299758539));
#11177=CARTESIAN_POINT('Ctrl Pts',(4.3,1.37908752581626,0.605290299758539));
#11178=CARTESIAN_POINT('Ctrl Pts',(3.23367147240841,1.34448060345116,0.605309774863278));
#11179=CARTESIAN_POINT('Ctrl Pts',(2.16694388170711,1.31755402957363,0.605319894542965));
#11180=CARTESIAN_POINT('Ctrl Pts',(1.10000000298281,1.29254692760111,0.605334652628557));
#11181=CARTESIAN_POINT('Ctrl Pts',(1.07338415738705,1.32427529283227,-8.86713457716078E-5));
#11182=CARTESIAN_POINT('Ctrl Pts',(1.08225606990759,1.31369916974318,0.201719104823349));
#11183=CARTESIAN_POINT('Ctrl Pts',(1.09112801825728,1.30312304798912,0.403526879488635));
#11184=CARTESIAN_POINT('Ctrl Pts',(1.10000000295732,1.29254692759565,0.605334652628532));
#11185=CARTESIAN_POINT('Ctrl Pts',(2.14856196511707,1.34935185539717,-5.92140853224782E-5));
#11186=CARTESIAN_POINT('Ctrl Pts',(2.15571155670469,1.33877574824882,0.201748609776328));
#11187=CARTESIAN_POINT('Ctrl Pts',(2.16286118630166,1.32819964054013,0.403556432267816));
#11188=CARTESIAN_POINT('Ctrl Pts',(2.17001085376486,1.31762353633116,0.605364253566666));
#11189=CARTESIAN_POINT('Ctrl Pts',(3.22410085073147,1.37636920007789,-3.90459518899617E-5));
#11190=CARTESIAN_POINT('Ctrl Pts',(3.22952869941811,1.36579313421484,0.201768811381317));
#11191=CARTESIAN_POINT('Ctrl Pts',(3.23495659078338,1.35521706809945,0.403576667516948));
#11192=CARTESIAN_POINT('Ctrl Pts',(3.24038452463064,1.34464100578453,0.605384522622892));
#11193=CARTESIAN_POINT('Ctrl Pts',(4.3,1.41116952203211,-1.07899800205757E-15));
#11194=CARTESIAN_POINT('Ctrl Pts',(4.3037066798556,1.40059355144758,0.201807922462832));
#11195=CARTESIAN_POINT('Ctrl Pts',(4.30741340932897,1.39001758331339,0.403615844145277));
#11196=CARTESIAN_POINT('Ctrl Pts',(4.31112018914115,1.37944161767694,0.605423765036611));
#11197=CARTESIAN_POINT('Origin',(0.9,1.39290118819044,0.));
#11198=CARTESIAN_POINT('',(0.900000001878204,-1.28788040994396,0.605337476551879));
#11199=CARTESIAN_POINT('Ctrl Pts',(0.900000001878204,-1.28788040994396,
0.605337476551879));
#11200=CARTESIAN_POINT('Ctrl Pts',(0.900000001878204,-1.29328625806092,
0.504228160928694));
#11201=CARTESIAN_POINT('Ctrl Pts',(0.899999999999999,-1.29869191435855,
0.403118132397745));
#11202=CARTESIAN_POINT('Ctrl Pts',(0.899999999999999,-1.30947917558554,
0.201339438823693));
#11203=CARTESIAN_POINT('Ctrl Pts',(0.9,-1.31486085669789,0.100669384150719));
#11204=CARTESIAN_POINT('Ctrl Pts',(0.9,-1.32024227787037,0.));
#11205=CARTESIAN_POINT('',(0.9,-1.18799600975353,0.7));
#11206=CARTESIAN_POINT('Ctrl Pts',(0.900000000000324,-1.18799600975363,
0.7));
#11207=CARTESIAN_POINT('Ctrl Pts',(0.900000000063601,-1.19590581948314,
0.699999999935493));
#11208=CARTESIAN_POINT('Ctrl Pts',(0.900000451671414,-1.20375274583281,
0.699006541951706));
#11209=CARTESIAN_POINT('Ctrl Pts',(0.900000834722547,-1.21139610511184,
0.697120084132161));
#11210=CARTESIAN_POINT('Ctrl Pts',(0.900001049758257,-1.21568690349652,
0.696061072005504));
#11211=CARTESIAN_POINT('Ctrl Pts',(0.900001241882928,-1.21991360580594,
0.694719604949841));
#11212=CARTESIAN_POINT('Ctrl Pts',(0.900001357948449,-1.22404965357203,
0.693106547509926));
#11213=CARTESIAN_POINT('Ctrl Pts',(0.900001566283472,-1.23147376710855,
0.690211145364658));
#11214=CARTESIAN_POINT('Ctrl Pts',(0.900001483882417,-1.23852542365708,
0.686475281350474));
#11215=CARTESIAN_POINT('Ctrl Pts',(0.90000115772027,-1.24505817055452,0.681980323292531));
#11216=CARTESIAN_POINT('Ctrl Pts',(0.90000097852015,-1.2486473946309,0.67951070187031));
#11217=CARTESIAN_POINT('Ctrl Pts',(0.900000731874511,-1.25207971535834,
0.676811055842604));
#11218=CARTESIAN_POINT('Ctrl Pts',(0.90000051586667,-1.25532695882913,0.673889369778116));
#11219=CARTESIAN_POINT('Ctrl Pts',(0.900000304282776,-1.25850769714062,
0.671027521295527));
#11220=CARTESIAN_POINT('Ctrl Pts',(0.900000119565725,-1.26149151526032,
0.667969976014938));
#11221=CARTESIAN_POINT('Ctrl Pts',(0.900000124706954,-1.26425564062679,
0.664728268702146));
#11222=CARTESIAN_POINT('Ctrl Pts',(0.900000134210909,-1.26936533657602,
0.658735726205464));
#11223=CARTESIAN_POINT('Ctrl Pts',(0.900000724431276,-1.2737272220214,0.652115259198653));
#11224=CARTESIAN_POINT('Ctrl Pts',(0.900000949945503,-1.27728244659665,
0.645033014705304));
#11225=CARTESIAN_POINT('Ctrl Pts',(0.900000972753073,-1.27764200720725,
0.644316745985709));
#11226=CARTESIAN_POINT('Ctrl Pts',(0.900000992743332,-1.27799327761064,
0.64359573459864));
#11227=CARTESIAN_POINT('Ctrl Pts',(0.900001009576454,-1.27833616945273,
0.642870141642621));
#11228=CARTESIAN_POINT('Ctrl Pts',(0.900001176059944,-1.28172744954266,
0.635693858502874));
#11229=CARTESIAN_POINT('Ctrl Pts',(0.900000930108723,-1.28426399347052,
0.628153947608977));
#11230=CARTESIAN_POINT('Ctrl Pts',(0.900000539908504,-1.2858931319598,0.620419547606466));
#11231=CARTESIAN_POINT('Ctrl Pts',(0.900000289636433,-1.28693805157347,
0.615458750034127));
#11232=CARTESIAN_POINT('Ctrl Pts',(0.900000000000001,-1.28760881677759,
0.610417269724172));
#11233=CARTESIAN_POINT('Ctrl Pts',(0.900000000000001,-1.28788040985668,
0.605337476551933));
#11234=CARTESIAN_POINT('',(0.9,1.18799600975353,0.7));
#11235=CARTESIAN_POINT('',(0.9,0.696450594095222,0.7));
#11236=CARTESIAN_POINT('',(0.900000001878204,1.28788040994396,0.605337476551879));
#11237=CARTESIAN_POINT('Ctrl Pts',(0.900000000000001,1.28788040985668,0.605337476551933));
#11238=CARTESIAN_POINT('Ctrl Pts',(0.900000000000001,1.28745726486871,0.613251849878237));
#11239=CARTESIAN_POINT('Ctrl Pts',(0.900000641820462,1.28606767879774,0.621075732439556));
#11240=CARTESIAN_POINT('Ctrl Pts',(0.900000906166769,1.28379497466322,0.628648019961568));
#11241=CARTESIAN_POINT('Ctrl Pts',(0.900001053446495,1.2825287445946,0.632866896498568));
#11242=CARTESIAN_POINT('Ctrl Pts',(0.900001106693909,1.28098738700664,0.637007708770872));
#11243=CARTESIAN_POINT('Ctrl Pts',(0.900001044867119,1.27917862712792,0.641040603354488));
#11244=CARTESIAN_POINT('Ctrl Pts',(0.900000933962191,1.27593407274945,0.64827481168313));
#11245=CARTESIAN_POINT('Ctrl Pts',(0.900000399592996,1.27186725264719,0.655083885116145));
#11246=CARTESIAN_POINT('Ctrl Pts',(0.900000190596867,1.2670411556595,0.661303993035384));
#11247=CARTESIAN_POINT('Ctrl Pts',(0.900000151538061,1.26613921747962,0.662466454716044));
#11248=CARTESIAN_POINT('Ctrl Pts',(0.900000126821978,1.26521063179286,0.663608275427336));
#11249=CARTESIAN_POINT('Ctrl Pts',(0.900000125264574,1.26425564063975,0.664728268702142));
#11250=CARTESIAN_POINT('Ctrl Pts',(0.90000012217056,1.26235840892454,0.66695330163032));
#11251=CARTESIAN_POINT('Ctrl Pts',(0.900000209712012,1.26035699384613,0.66909223571964));
#11252=CARTESIAN_POINT('Ctrl Pts',(0.900000331194293,1.2582587086698,0.671141334714948));
#11253=CARTESIAN_POINT('Ctrl Pts',(0.900000660246931,1.25257519443757,0.676691620936499));
#11254=CARTESIAN_POINT('Ctrl Pts',(0.900001184896248,1.24624785575673,0.681523125886843));
#11255=CARTESIAN_POINT('Ctrl Pts',(0.900001377531805,1.23944073409582,0.685581770965975));
#11256=CARTESIAN_POINT('Ctrl Pts',(0.900001499905572,1.2351164383281,0.68816006802201));
#11257=CARTESIAN_POINT('Ctrl Pts',(0.900001510509735,1.23059756718463,0.690425789971136));
#11258=CARTESIAN_POINT('Ctrl Pts',(0.900001405318139,1.22592052877826,0.692355791713551));
#11259=CARTESIAN_POINT('Ctrl Pts',(0.900001240727996,1.21860250674997,0.695375607682216));
#11260=CARTESIAN_POINT('Ctrl Pts',(0.900000792095824,1.21098234272326,0.697541065921879));
#11261=CARTESIAN_POINT('Ctrl Pts',(0.900000425437202,1.20320741268883,0.698782789564668));
#11262=CARTESIAN_POINT('Ctrl Pts',(0.900000188792485,1.19818940410026,0.699584208982791));
#11263=CARTESIAN_POINT('Ctrl Pts',(0.900000000041206,1.19310633605572,0.699999999958324));
#11264=CARTESIAN_POINT('Ctrl Pts',(0.900000000000325,1.18799600975363,0.7));
#11265=CARTESIAN_POINT('Ctrl Pts',(0.9,1.32024227787037,0.));
#11266=CARTESIAN_POINT('Ctrl Pts',(0.9,1.31486080448354,0.100670360916234));
#11267=CARTESIAN_POINT('Ctrl Pts',(0.9,1.30947907114291,0.201341392534));
#11268=CARTESIAN_POINT('Ctrl Pts',(0.9,1.2986918099064,0.403120086121531));
#11269=CARTESIAN_POINT('Ctrl Pts',(0.900000001878204,1.29328620583358,0.504229137772713));
#11270=CARTESIAN_POINT('Ctrl Pts',(0.900000001878204,1.28788040994396,0.605337476551879));
#11271=CARTESIAN_POINT('Ctrl Pts',(0.899999999999997,-1.32024227787137,
-1.86669707469278E-11));
#11272=CARTESIAN_POINT('Ctrl Pts',(0.909148787559422,-1.30966717532842,
0.201788252636133));
#11273=CARTESIAN_POINT('Ctrl Pts',(0.91829761066914,-1.29909207410335,0.403576503749508));
#11274=CARTESIAN_POINT('Ctrl Pts',(0.92744646984625,-1.28851697422138,0.605364753299354));
#11275=CARTESIAN_POINT('Ctrl Pts',(0.699273108318574,-1.31559634352334,
-5.7001548815619E-6));
#11276=CARTESIAN_POINT('Ctrl Pts',(0.708743431409066,-1.30502123870946,
0.20178254329682));
#11277=CARTESIAN_POINT('Ctrl Pts',(0.718213789763005,-1.2944461351935,0.403570785162392));
#11278=CARTESIAN_POINT('Ctrl Pts',(0.727684183892774,-1.28387103300525,
0.605359025419352));
#11279=CARTESIAN_POINT('Ctrl Pts',(0.498558799217305,-1.31100715552056,
-1.1774619888836E-5));
#11280=CARTESIAN_POINT('Ctrl Pts',(0.508350677965937,-1.30043204942944,
0.201776459055217));
#11281=CARTESIAN_POINT('Ctrl Pts',(0.518142591787393,-1.28985694462582,
0.403564691096996));
#11282=CARTESIAN_POINT('Ctrl Pts',(0.527934541191295,-1.27928184113929,
0.60535292148228));
#11283=CARTESIAN_POINT('Ctrl Pts',(0.29785707328833,-1.3064367443434,-1.84041486642056E-5));
#11284=CARTESIAN_POINT('Ctrl Pts',(0.307970527825607,-1.29586163794,0.20176981888596));
#11285=CARTESIAN_POINT('Ctrl Pts',(0.318084017341356,-1.28528653282298,
0.403558040236175));
#11286=CARTESIAN_POINT('Ctrl Pts',(0.328197542344371,-1.27471142901691,
0.605346259877786));
#11287=CARTESIAN_POINT('',(0.32957180616905,-1.2747428754212,0.605346305703265));
#11288=CARTESIAN_POINT('Ctrl Pts',(0.297857995688647,-1.306435779838,1.57426155444895E-16));
#11289=CARTESIAN_POINT('Ctrl Pts',(0.308429283449307,-1.29587142805659,
0.201782098465301));
#11290=CARTESIAN_POINT('Ctrl Pts',(0.319000553694994,-1.28530712634462,
0.403564200350135));
#11291=CARTESIAN_POINT('Ctrl Pts',(0.329571806169048,-1.2747428754212,0.605346305703266));
#11292=CARTESIAN_POINT('Ctrl Pts',(0.32957180616905,-1.2747428754212,0.605346305703265));
#11293=CARTESIAN_POINT('Ctrl Pts',(0.519721397561595,-1.27909449722757,
0.60534313598158));
#11294=CARTESIAN_POINT('Ctrl Pts',(0.709864288600121,-1.28346276435313,
0.605340219076093));
#11295=CARTESIAN_POINT('Ctrl Pts',(0.900000001879218,-1.28788040990034,
0.605337476551906));
#11296=CARTESIAN_POINT('Ctrl Pts',(0.90231940407953,-1.18804989493878,0.7));
#11297=CARTESIAN_POINT('Ctrl Pts',(0.712166351817731,-1.18363199317816,
0.7));
#11298=CARTESIAN_POINT('Ctrl Pts',(0.522011847238247,-1.17926361631973,
0.7));
#11299=CARTESIAN_POINT('Ctrl Pts',(0.331856371369203,-1.17491202960101,
0.7));
#11300=CARTESIAN_POINT('Ctrl Pts',(0.901648075315333,-1.21694488185794,
0.7));
#11301=CARTESIAN_POINT('Ctrl Pts',(0.711500071980331,-1.21252656425213,
0.69999998041973));
#11302=CARTESIAN_POINT('Ctrl Pts',(0.521348914609444,-1.20815772874132,
0.700000022626678));
#11303=CARTESIAN_POINT('Ctrl Pts',(0.331195161244126,-1.20380556524924,
0.7));
#11304=CARTESIAN_POINT('Ctrl Pts',(0.900484091294294,-1.26704448261357,
0.676664431332699));
#11305=CARTESIAN_POINT('Ctrl Pts',(0.710344780071471,-1.26262550764723,
0.676665329845182));
#11306=CARTESIAN_POINT('Ctrl Pts',(0.520199507967113,-1.25825584722226,
0.676666267597974));
#11307=CARTESIAN_POINT('Ctrl Pts',(0.3300487189482,-1.25390275839508,0.676667306001616));
#11308=CARTESIAN_POINT('Ctrl Pts',(0.90002687589075,-1.28672371253673,0.626983665342106));
#11309=CARTESIAN_POINT('Ctrl Pts',(0.709890987426059,-1.28230548388611,
0.626985988983916));
#11310=CARTESIAN_POINT('Ctrl Pts',(0.519747959090447,-1.27793661492756,
0.626988445273931));
#11311=CARTESIAN_POINT('Ctrl Pts',(0.329598318905021,-1.27358432286302,
0.626991130804315));
#11312=CARTESIAN_POINT('Ctrl Pts',(0.900000001879218,-1.28788040990034,
0.605337476551906));
#11313=CARTESIAN_POINT('Ctrl Pts',(0.709864288600121,-1.28346276435313,
0.605340219076093));
#11314=CARTESIAN_POINT('Ctrl Pts',(0.519721397561595,-1.27909449722757,
0.60534313598158));
#11315=CARTESIAN_POINT('Ctrl Pts',(0.32957180616905,-1.2747428754212,0.605346305703265));
#11316=CARTESIAN_POINT('',(0.331856371369201,-1.17491202962433,0.7));
#11317=CARTESIAN_POINT('Origin',(0.331856371539144,-1.1749120296049,0.6));
#11318=CARTESIAN_POINT('Ctrl Pts',(0.900000000000328,-1.18799600975363,
0.7));
#11319=CARTESIAN_POINT('Ctrl Pts',(0.71062007065371,-1.18359647108512,0.7));
#11320=CARTESIAN_POINT('Ctrl Pts',(0.521238702715143,-1.17924592340069,
0.7));
#11321=CARTESIAN_POINT('Ctrl Pts',(0.331856371369203,-1.17491202960101,
0.7));
#11322=CARTESIAN_POINT('Origin',(6.87409734069396,-2.22251806091942E-16,
0.7));
#11323=CARTESIAN_POINT('',(0.331856371879032,1.17491202961268,0.7));
#11324=CARTESIAN_POINT('',(0.331856371369201,-0.75,0.7));
#11325=CARTESIAN_POINT('Ctrl Pts',(0.331856371879031,1.17491202961268,0.7));
#11326=CARTESIAN_POINT('Ctrl Pts',(0.521238703055026,1.1792459234085,0.7));
#11327=CARTESIAN_POINT('Ctrl Pts',(0.710620070823648,1.18359647108907,0.7));
#11328=CARTESIAN_POINT('Ctrl Pts',(0.900000000000325,1.18799600975363,0.7));
#11329=CARTESIAN_POINT('Ctrl Pts',(0.297857073289265,1.30643674434242,-1.84041299971672E-5));
#11330=CARTESIAN_POINT('Ctrl Pts',(0.30797052782623,1.29586163793935,0.201769818898405));
#11331=CARTESIAN_POINT('Ctrl Pts',(0.318084017341667,1.28528653282265,0.403558040242397));
#11332=CARTESIAN_POINT('Ctrl Pts',(0.328197542344371,1.27471142901691,0.605346259877786));
#11333=CARTESIAN_POINT('Ctrl Pts',(0.49855879921793,1.31100715551957,-1.17746012218085E-5));
#11334=CARTESIAN_POINT('Ctrl Pts',(0.50835067796626,1.30043204942878,0.201776459067662));
#11335=CARTESIAN_POINT('Ctrl Pts',(0.518142591787414,1.28985694462549,0.403564691103219));
#11336=CARTESIAN_POINT('Ctrl Pts',(0.527934541191015,1.27928184113928,0.60535292148228));
#11337=CARTESIAN_POINT('Ctrl Pts',(0.699273108318888,1.31559634352235,-5.70013621459206E-6));
#11338=CARTESIAN_POINT('Ctrl Pts',(0.708743431409089,1.3050212387088,0.201782543309265));
#11339=CARTESIAN_POINT('Ctrl Pts',(0.718213789762737,1.29444613519316,0.403570785168614));
#11340=CARTESIAN_POINT('Ctrl Pts',(0.727684183892215,1.28387103300524,0.605359025419352));
#11341=CARTESIAN_POINT('Ctrl Pts',(0.9,1.32024227787037,-6.93889390390723E-18));
#11342=CARTESIAN_POINT('Ctrl Pts',(0.909148787559144,1.30966717532775,0.201788252648578));
#11343=CARTESIAN_POINT('Ctrl Pts',(0.918297610668582,1.29909207410301,0.403576503755731));
#11344=CARTESIAN_POINT('Ctrl Pts',(0.927446469845411,1.28851697422136,0.605364753299355));
#11345=CARTESIAN_POINT('',(0.329571806169048,1.2747428754212,0.605346305703265));
#11346=CARTESIAN_POINT('Ctrl Pts',(0.900000001879216,1.28788040990034,0.605337476551906));
#11347=CARTESIAN_POINT('Ctrl Pts',(0.709864288600119,1.28346276435313,0.605340219076093));
#11348=CARTESIAN_POINT('Ctrl Pts',(0.519721397561593,1.27909449722757,0.60534313598158));
#11349=CARTESIAN_POINT('Ctrl Pts',(0.329571806169048,1.2747428754212,0.605346305703265));
#11350=CARTESIAN_POINT('Ctrl Pts',(0.329571806169048,1.2747428754212,0.605346305703265));
#11351=CARTESIAN_POINT('Ctrl Pts',(0.319000553694994,1.28530712634462,0.403564200350134));
#11352=CARTESIAN_POINT('Ctrl Pts',(0.308429283449307,1.29587142805659,0.201782098465301));
#11353=CARTESIAN_POINT('Ctrl Pts',(0.297857995688647,1.306435779838,6.03900610074426E-17));
#11354=CARTESIAN_POINT('Ctrl Pts',(0.331856371369201,1.17491202960101,0.7));
#11355=CARTESIAN_POINT('Ctrl Pts',(0.522011847238246,1.17926361631973,0.7));
#11356=CARTESIAN_POINT('Ctrl Pts',(0.712166351817729,1.18363199317816,0.7));
#11357=CARTESIAN_POINT('Ctrl Pts',(0.902319404079528,1.18804989493878,0.7));
#11358=CARTESIAN_POINT('Ctrl Pts',(0.331195161244124,1.20380556524924,0.7));
#11359=CARTESIAN_POINT('Ctrl Pts',(0.521348914609443,1.20815772874132,0.700000022626678));
#11360=CARTESIAN_POINT('Ctrl Pts',(0.711500071980329,1.21252656425213,0.69999998041973));
#11361=CARTESIAN_POINT('Ctrl Pts',(0.901648075315331,1.21694488185794,0.7));
#11362=CARTESIAN_POINT('Ctrl Pts',(0.330048718948197,1.25390275839508,0.676667306001616));
#11363=CARTESIAN_POINT('Ctrl Pts',(0.52019950796711,1.25825584722226,0.676666267597973));
#11364=CARTESIAN_POINT('Ctrl Pts',(0.710344780071469,1.26262550764723,0.676665329845182));
#11365=CARTESIAN_POINT('Ctrl Pts',(0.900484091294292,1.26704448261357,0.676664431332698));
#11366=CARTESIAN_POINT('Ctrl Pts',(0.329598318905018,1.27358432286302,0.626991130804315));
#11367=CARTESIAN_POINT('Ctrl Pts',(0.519747959090446,1.27793661492756,0.62698844527393));
#11368=CARTESIAN_POINT('Ctrl Pts',(0.709890987426057,1.28230548388611,0.626985988983916));
#11369=CARTESIAN_POINT('Ctrl Pts',(0.900026875890748,1.28672371253673,0.626983665342106));
#11370=CARTESIAN_POINT('Ctrl Pts',(0.329571806169048,1.2747428754212,0.605346305703265));
#11371=CARTESIAN_POINT('Ctrl Pts',(0.519721397561593,1.27909449722757,0.60534313598158));
#11372=CARTESIAN_POINT('Ctrl Pts',(0.709864288600119,1.28346276435313,0.605340219076093));
#11373=CARTESIAN_POINT('Ctrl Pts',(0.900000001879216,1.28788040990034,0.605337476551906));
#11374=CARTESIAN_POINT('Origin',(0.331856371369202,1.17491202960101,0.6));
#11375=CARTESIAN_POINT('Origin',(0.331856371369202,1.17491202960101,0.6));
#11376=CARTESIAN_POINT('Origin',(0.331856371369201,1.17491202960879,0.6));
#11377=CARTESIAN_POINT('Origin',(0.331856371369202,1.17491202960101,0.6));
#11378=CARTESIAN_POINT('Origin',(12.8681436286308,1.83274446434879,0.6));
#11379=CARTESIAN_POINT('Origin',(12.8681436286308,1.83274446434879,0.6));
#11380=CARTESIAN_POINT('',(12.9680065821063,1.83274446434879,0.605233595624294));
#11381=CARTESIAN_POINT('Origin',(12.8681436286308,1.83274446434879,0.6));
#11382=CARTESIAN_POINT('Origin',(12.8681436286308,1.83274446434879,0.6));
#11383=CARTESIAN_POINT('Origin',(0.331856371369201,-1.17491202960101,0.6));
#11384=CARTESIAN_POINT('Origin',(0.331856371369201,-1.17491202960101,0.6));
#11385=CARTESIAN_POINT('Origin',(0.331856371369201,-1.17491202960101,0.6));
#11386=CARTESIAN_POINT('Origin',(0.331856371369201,-0.75,0.6));
#11387=CARTESIAN_POINT('Ctrl Pts',(0.297750759617602,-1.30654294555098,
-0.00204689530870639));
#11388=CARTESIAN_POINT('Ctrl Pts',(0.308357792853923,-1.29594287152607,
0.200417501569666));
#11389=CARTESIAN_POINT('Ctrl Pts',(0.318964808457496,-1.28534284790734,
0.40288190189057));
#11390=CARTESIAN_POINT('Ctrl Pts',(0.329571806169048,-1.2747428754212,0.605346305703266));
#11391=CARTESIAN_POINT('Ctrl Pts',(0.268364475985512,-1.30579334864515,
-0.000546070465277405));
#11392=CARTESIAN_POINT('Ctrl Pts',(0.278972236061358,-1.29519218153762,
0.201918231169276));
#11393=CARTESIAN_POINT('Ctrl Pts',(0.289579970322816,-1.28459115545203,
0.404382541571378));
#11394=CARTESIAN_POINT('Ctrl Pts',(0.300187702091134,-1.27399007937578,
0.606846849214128));
#11395=CARTESIAN_POINT('Ctrl Pts',(0.217994620733579,-1.28028753054242,
0.000758348866131992));
#11396=CARTESIAN_POINT('Ctrl Pts',(0.228604439653725,-1.26968580576698,
0.203222517770204));
#11397=CARTESIAN_POINT('Ctrl Pts',(0.239214264875756,-1.259084092946,0.405686686833815));
#11398=CARTESIAN_POINT('Ctrl Pts',(0.24982407554016,-1.24848245399652,0.608150860486448));
#11399=CARTESIAN_POINT('Ctrl Pts',(0.200221638751335,-1.22875730734246,
-0.00100806500432267));
#11400=CARTESIAN_POINT('Ctrl Pts',(0.210832346469089,-1.21815680658782,
0.201456130081263));
#11401=CARTESIAN_POINT('Ctrl Pts',(0.221443027663539,-1.20755634130466,
0.403920328365886));
#11402=CARTESIAN_POINT('Ctrl Pts',(0.232053735729819,-1.1969559383274,0.606384528499152));
#11403=CARTESIAN_POINT('Ctrl Pts',(0.200161316008396,-1.20671181983024,
-0.00215909150772397));
#11404=CARTESIAN_POINT('Ctrl Pts',(0.21077201649647,-1.19611183845239,0.200305134857769));
#11405=CARTESIAN_POINT('Ctrl Pts',(0.221382717124246,-1.18551190812967,
0.402769363888924));
#11406=CARTESIAN_POINT('Ctrl Pts',(0.231993417893744,-1.17491202960101,
0.605233595624295));
#11407=CARTESIAN_POINT('Origin',(12.8681436286308,-1.83274446434879,0.6));
#11408=CARTESIAN_POINT('',(12.9680065821063,-1.83274446434879,0.605233595624295));
#11409=CARTESIAN_POINT('Origin',(12.8681436286308,-1.83274446434879,0.6));
#11410=CARTESIAN_POINT('Origin',(12.8681436286308,-1.83274446434879,0.6));
#11411=CARTESIAN_POINT('Origin',(12.8681436286308,1.1,0.6));
#11412=CARTESIAN_POINT('',(12.9680065821063,1.1,0.605233595624295));
#11413=CARTESIAN_POINT('Ctrl Pts',(12.9998428721614,-1.86475648739599,-0.00223900654757928));
#11414=CARTESIAN_POINT('Ctrl Pts',(12.9892307746816,-1.85408610159386,0.200251876006837));
#11415=CARTESIAN_POINT('Ctrl Pts',(12.9786186779927,-1.84341542867022,0.402742743472647));
#11416=CARTESIAN_POINT('Ctrl Pts',(12.9680065821063,-1.83274446434879,0.605233595624296));
#11417=CARTESIAN_POINT('Ctrl Pts',(12.9997989521977,-1.88070362541494,-0.00140096371806573));
#11418=CARTESIAN_POINT('Ctrl Pts',(12.9891868560404,-1.87003481788623,0.2010900171988));
#11419=CARTESIAN_POINT('Ctrl Pts',(12.9785747412344,-1.85936572080465,0.403580981971657));
#11420=CARTESIAN_POINT('Ctrl Pts',(12.967962646681,-1.84869634914788,0.606071933479074));
#11421=CARTESIAN_POINT('Ctrl Pts',(12.9919061104719,-1.91252097257855,-0.00013797468654593));
#11422=CARTESIAN_POINT('Ctrl Pts',(12.9812924311808,-1.9018552985481,0.202353118580234));
#11423=CARTESIAN_POINT('Ctrl Pts',(12.970678744243,-1.89118929884075,0.404844194499128));
#11424=CARTESIAN_POINT('Ctrl Pts',(12.9600650516023,-1.88052308923615,0.607335259545336));
#11425=CARTESIAN_POINT('Ctrl Pts',(12.9539932318948,-1.95585643963679,0.000158685530800887));
#11426=CARTESIAN_POINT('Ctrl Pts',(12.9433725220626,-1.94519261899951,0.202649549046396));
#11427=CARTESIAN_POINT('Ctrl Pts',(12.9327517623504,-1.93452853669393,0.40514039680648));
#11428=CARTESIAN_POINT('Ctrl Pts',(12.9221309734579,-1.92386419524738,0.607631230057729));
#11429=CARTESIAN_POINT('Ctrl Pts',(12.9129235702791,-1.96658826742031,-0.00142816374191492));
#11430=CARTESIAN_POINT('Ctrl Pts',(12.9022969271978,-1.95592037993921,0.201062184830579));
#11431=CARTESIAN_POINT('Ctrl Pts',(12.891670251582,-1.94525202616943,0.403552507423554));
#11432=CARTESIAN_POINT('Ctrl Pts',(12.8810434760214,-1.93458357684419,0.60604282089977));
#11433=CARTESIAN_POINT('Ctrl Pts',(12.8891437477602,-1.96405813112492,-0.00280773857265357));
#11434=CARTESIAN_POINT('Ctrl Pts',(12.8785151960038,-1.95338599020215,0.199682283294402));
#11435=CARTESIAN_POINT('Ctrl Pts',(12.8678865709412,-1.94271355010484,0.402172286243574));
#11436=CARTESIAN_POINT('Ctrl Pts',(12.8572578715866,-1.93204080633595,0.604662269998931));
#11437=CARTESIAN_POINT('Ctrl Pts',(12.9997255308004,-1.86463850151065,-4.9439619065339E-17));
#11438=CARTESIAN_POINT('Ctrl Pts',(12.9891525471135,-1.85400744222428,0.201744546927532));
#11439=CARTESIAN_POINT('Ctrl Pts',(12.9785795642115,-1.84337609791338,0.403489078876654));
#11440=CARTESIAN_POINT('Ctrl Pts',(12.9680065821063,-1.83274446434879,0.605233595624296));
#11441=CARTESIAN_POINT('Ctrl Pts',(12.8891409639924,1.96405533594058,-0.00275470357795049));
#11442=CARTESIAN_POINT('Ctrl Pts',(12.8785133401458,1.95338412669368,0.199717639954231));
#11443=CARTESIAN_POINT('Ctrl Pts',(12.8678856430057,1.9427126183241,0.402189964571813));
#11444=CARTESIAN_POINT('Ctrl Pts',(12.8572578715866,1.93204080633595,0.604662269998929));
#11445=CARTESIAN_POINT('Ctrl Pts',(12.9049941793403,1.96574209420267,-0.00183498696757459));
#11446=CARTESIAN_POINT('Ctrl Pts',(12.8943678341644,1.95507368670196,0.20063757283533));
#11447=CARTESIAN_POINT('Ctrl Pts',(12.8837414238008,1.94440496992476,0.403110113573296));
#11448=CARTESIAN_POINT('Ctrl Pts',(12.8731149412098,1.93373598667478,0.605582637266155));
#11449=CARTESIAN_POINT('Ctrl Pts',(12.9374710816243,1.9613461313261,-0.000364592700753267));
#11450=CARTESIAN_POINT('Ctrl Pts',(12.9268487371951,1.95068187676899,0.202108391447626));
#11451=CARTESIAN_POINT('Ctrl Pts',(12.9162262930262,1.94001732715406,0.404581355450702));
#11452=CARTESIAN_POINT('Ctrl Pts',(12.9056038462248,1.92935253789361,0.607054307450502));
#11453=CARTESIAN_POINT('Ctrl Pts',(12.9846523118271,1.92834870343354,0.000369250346899581));
#11454=CARTESIAN_POINT('Ctrl Pts',(12.974038022963,1.91768545846127,0.202842678583437));
#11455=CARTESIAN_POINT('Ctrl Pts',(12.9634237233674,1.90702194269714,0.405316092420461));
#11456=CARTESIAN_POINT('Ctrl Pts',(12.9528094065597,1.89635817580376,0.607789492622546));
#11457=CARTESIAN_POINT('Ctrl Pts',(12.9997742127558,1.88867440031858,-0.000928907044737527));
#11458=CARTESIAN_POINT('Ctrl Pts',(12.9891630904765,1.8780073281596,0.201544447891303));
#11459=CARTESIAN_POINT('Ctrl Pts',(12.9785517991681,1.86733992038445,0.404017776344753));
#11460=CARTESIAN_POINT('Ctrl Pts',(12.9679406789684,1.85667229154743,0.606491102406462));
#11461=CARTESIAN_POINT('Ctrl Pts',(12.9998400927033,1.86475369267134,-0.00218597132744988));
#11462=CARTESIAN_POINT('Ctrl Pts',(12.9892289217097,1.85408423839396,0.200287232817622));
#11463=CARTESIAN_POINT('Ctrl Pts',(12.9786177515068,1.84341449704483,0.402760421876702));
#11464=CARTESIAN_POINT('Ctrl Pts',(12.9680065821063,1.83274446434879,0.605233595624294));
#11465=CARTESIAN_POINT('Ctrl Pts',(12.9680065821063,1.83274446434879,0.605233595624294));
#11466=CARTESIAN_POINT('Ctrl Pts',(12.9785795642115,1.84337609791338,0.403489078876654));
#11467=CARTESIAN_POINT('Ctrl Pts',(12.9891525471135,1.85400744222428,0.201744546927532));
#11468=CARTESIAN_POINT('Ctrl Pts',(12.9997255308004,1.86463850151065,1.86916454536501E-16));
#11469=CARTESIAN_POINT('Ctrl Pts',(12.6,1.80383022254432,0.7));
#11470=CARTESIAN_POINT('Ctrl Pts',(12.6893984576578,1.8133105623702,0.7));
#11471=CARTESIAN_POINT('Ctrl Pts',(12.7787800350189,1.82294762441299,0.7));
#11472=CARTESIAN_POINT('Ctrl Pts',(12.8681436286308,1.83274446434879,0.7));
#11473=CARTESIAN_POINT('Ctrl Pts',(12.5969393303222,1.83269196733649,0.7));
#11474=CARTESIAN_POINT('Ctrl Pts',(12.686303642571,1.84217134991284,0.700000098415946));
#11475=CARTESIAN_POINT('Ctrl Pts',(12.7756511334299,1.85180730951691,0.699999896874207));
#11476=CARTESIAN_POINT('Ctrl Pts',(12.8649798835675,1.86160311979107,0.7));
#11477=CARTESIAN_POINT('Ctrl Pts',(12.5916356538948,1.88270499442536,0.67643906321291));
#11478=CARTESIAN_POINT('Ctrl Pts',(12.6809412203008,1.89218243450198,0.676434576658958));
#11479=CARTESIAN_POINT('Ctrl Pts',(12.7702288461642,1.90181652272411,0.676430055978541));
#11480=CARTESIAN_POINT('Ctrl Pts',(12.8594976525144,1.91161025179704,0.676425356750174));
#11481=CARTESIAN_POINT('Ctrl Pts',(12.58957419749,1.90214427893475,0.626447702441804));
#11482=CARTESIAN_POINT('Ctrl Pts',(12.6788572782758,1.91161594713488,0.626436135819418));
#11483=CARTESIAN_POINT('Ctrl Pts',(12.7681225846323,1.92124403769089,0.626424372515079));
#11484=CARTESIAN_POINT('Ctrl Pts',(12.8573684983393,1.93103170500986,0.626412260100396));
#11485=CARTESIAN_POINT('Ctrl Pts',(12.5894662143615,1.90316254677271,0.604704117718382));
#11486=CARTESIAN_POINT('Ctrl Pts',(12.6787484942245,1.91263121188366,0.60469048808123));
#11487=CARTESIAN_POINT('Ctrl Pts',(12.7680127446979,1.92225628370762,0.604676541242762));
#11488=CARTESIAN_POINT('Ctrl Pts',(12.8572578715866,1.93204080633595,0.60466226999893));
#11489=CARTESIAN_POINT('Ctrl Pts',(0.200160815981423,1.20671231935208,-0.00216863259073552));
#11490=CARTESIAN_POINT('Ctrl Pts',(0.21077168314515,1.19611217146534,0.200298774135678));
#11491=CARTESIAN_POINT('Ctrl Pts',(0.221382550448584,1.18551207463533,0.402766183527835));
#11492=CARTESIAN_POINT('Ctrl Pts',(0.231993417893744,1.17491202960101,0.605233595624295));
#11493=CARTESIAN_POINT('Ctrl Pts',(0.200241246305444,1.23610630273461,-0.000633930584249493));
#11494=CARTESIAN_POINT('Ctrl Pts',(0.210852138766318,1.22550544237485,0.201833432539687));
#11495=CARTESIAN_POINT('Ctrl Pts',(0.221462948692539,1.21490467236247,0.404300804744641));
#11496=CARTESIAN_POINT('Ctrl Pts',(0.232073841675177,1.20430390790287,0.60676817279077));
#11497=CARTESIAN_POINT('Ctrl Pts',(0.224595236946023,1.28704077752974,0.000756396927320467));
#11498=CARTESIAN_POINT('Ctrl Pts',(0.235204871724134,1.27643877611169,0.203223757667495));
#11499=CARTESIAN_POINT('Ctrl Pts',(0.245814524913363,1.26583679641595,0.405691118453359));
#11500=CARTESIAN_POINT('Ctrl Pts',(0.256424148042823,1.25523487973404,0.608158484046399));
#11501=CARTESIAN_POINT('Ctrl Pts',(0.275710547013829,1.30598124743532,-0.000930817763883136));
#11502=CARTESIAN_POINT('Ctrl Pts',(0.286318282165364,1.29538020346814,0.201536689442792));
#11503=CARTESIAN_POINT('Ctrl Pts',(0.296926023167072,1.2847792285374,0.404004199876323));
#11504=CARTESIAN_POINT('Ctrl Pts',(0.307533728110612,1.27417827838713,0.606471713336412));
#11505=CARTESIAN_POINT('Ctrl Pts',(0.297750259763447,1.30654344507719,-0.0020564363997533));
#11506=CARTESIAN_POINT('Ctrl Pts',(0.308357459618374,1.29594320454196,0.200411140842193));
#11507=CARTESIAN_POINT('Ctrl Pts',(0.318964641840002,1.28534301441448,0.402878721526778));
#11508=CARTESIAN_POINT('Ctrl Pts',(0.329571806169048,1.2747428754212,0.605346305703265));
#11509=CARTESIAN_POINT('Origin',(13.0002740930491,2.2,-0.0104671912485888));
#11510=CARTESIAN_POINT('Origin',(0.331856371369202,1.17491202960101,0.6));
#11511=CARTESIAN_POINT('',(0.331856371879032,1.17491202961268,0.9));
#11512=CARTESIAN_POINT('',(0.0322675109428289,1.17491202960101,0.615700786872883));
#11513=CARTESIAN_POINT('Origin',(0.331856371369201,1.17491202962433,0.6));
#11514=CARTESIAN_POINT('',(0.325002675768741,1.47440456706157,0.616038917109795));
#11515=CARTESIAN_POINT('Origin',(0.331856371369202,1.17491202960101,0.6));
#11516=CARTESIAN_POINT('Origin',(0.331856371369201,1.17491202960101,0.6));
#11517=CARTESIAN_POINT('Origin',(12.8681436286308,1.83274446434879,0.6));
#11518=CARTESIAN_POINT('',(12.8681436286308,1.83274446434879,0.9));
#11519=CARTESIAN_POINT('',(12.8354863574981,2.13063349031027,0.613986809996789));
#11520=CARTESIAN_POINT('Origin',(12.8681436286308,1.83274446434879,0.6));
#11521=CARTESIAN_POINT('',(13.1677324890572,1.83274446434879,0.615700786872883));
#11522=CARTESIAN_POINT('Origin',(12.8681436286308,1.83274446434879,0.6));
#11523=CARTESIAN_POINT('Origin',(12.8681436286308,1.83274446434879,0.6));
#11524=CARTESIAN_POINT('Origin',(0.331856371369201,-1.17491202960101,0.6));
#11525=CARTESIAN_POINT('',(0.331856371369201,-1.17491202962433,0.9));
#11526=CARTESIAN_POINT('',(0.325002675768743,-1.47440456706157,0.616038917109795));
#11527=CARTESIAN_POINT('Origin',(0.331856371879032,-1.17491202961268,0.6));
#11528=CARTESIAN_POINT('',(0.0322675109428289,-1.17491202960101,0.615700786872884));
#11529=CARTESIAN_POINT('Origin',(0.331856371369201,-1.17491202960101,0.6));
#11530=CARTESIAN_POINT('Origin',(0.331856371369201,-1.17491202960101,0.6));
#11531=CARTESIAN_POINT('Origin',(0.331856371369201,-0.75,0.6));
#11532=CARTESIAN_POINT('',(0.0322675109428289,-0.75,0.615700786872883));
#11533=CARTESIAN_POINT('',(0.331856371369201,-0.75,0.9));
#11534=CARTESIAN_POINT('Ctrl Pts',(0.292429673212981,-1.5069793045954,-0.00614074949474724));
#11535=CARTESIAN_POINT('Ctrl Pts',(0.303287396789886,-1.49612100698918,
0.201252467440773));
#11536=CARTESIAN_POINT('Ctrl Pts',(0.314145064588525,-1.48526276089333,
0.408645689616972));
#11537=CARTESIAN_POINT('Ctrl Pts',(0.325002675768741,-1.47440456706157,
0.616038917109795));
#11538=CARTESIAN_POINT('Ctrl Pts',(0.204270663953122,-1.50473074636003,
-0.00163825452108868));
#11539=CARTESIAN_POINT('Ctrl Pts',(0.215130619942527,-1.49386909866124,
0.205754670272474));
#11540=CARTESIAN_POINT('Ctrl Pts',(0.225990497234893,-1.48300775583971,
0.413147615201549));
#11541=CARTESIAN_POINT('Ctrl Pts',(0.236850363534999,-1.47214617892531,
0.620540547642382));
#11542=CARTESIAN_POINT('Ctrl Pts',(0.0531014592841718,-1.42831231122466,
0.00228331220810075));
#11543=CARTESIAN_POINT('Ctrl Pts',(0.0639677431943945,-1.41744892560022,
0.209675827753147));
#11544=CARTESIAN_POINT('Ctrl Pts',(0.0748340498672138,-1.40658548887187,
0.417068339030394));
#11545=CARTESIAN_POINT('Ctrl Pts',(0.0857003072238147,-1.3957221574093,
0.624460858243749));
#11546=CARTESIAN_POINT('Ctrl Pts',(-0.000158492362241063,-1.27362248439808,
-0.0030242144278773));
#11547=CARTESIAN_POINT('Ctrl Pts',(0.0107105192099893,-1.2627628846508,
0.204368383073371));
#11548=CARTESIAN_POINT('Ctrl Pts',(0.0215794523842628,-1.25190326350425,
0.411760983371354));
#11549=CARTESIAN_POINT('Ctrl Pts',(0.0324484644510542,-1.24104375578019,
0.619153585497454));
#11550=CARTESIAN_POINT('Ctrl Pts',(-0.000339460947516079,-1.20748590713937,
-0.00647730073969574));
#11551=CARTESIAN_POINT('Ctrl Pts',(0.0105295295353408,-1.19662789414299,
0.200915392321314));
#11552=CARTESIAN_POINT('Ctrl Pts',(0.0213985201647323,-1.18576993469886,
0.408308088178364));
#11553=CARTESIAN_POINT('Ctrl Pts',(0.032267510942829,-1.17491202960101,
0.615700786872884));
#11554=CARTESIAN_POINT('Ctrl Pts',(0.292751161823634,-1.50665779898694,
4.33680868994202E-17));
#11555=CARTESIAN_POINT('Ctrl Pts',(0.30350172143464,-1.49590667092872,0.205346300540216));
#11556=CARTESIAN_POINT('Ctrl Pts',(0.314252226354851,-1.48515559337638,
0.410692606218909));
#11557=CARTESIAN_POINT('Ctrl Pts',(0.325002675768741,-1.47440456706157,
0.616038917109795));
#11558=CARTESIAN_POINT('Ctrl Pts',(0.032267510942829,-1.17491202960101,
0.615700786872884));
#11559=CARTESIAN_POINT('Ctrl Pts',(0.021511673816962,-1.18565689645617,
0.410467188483275));
#11560=CARTESIAN_POINT('Ctrl Pts',(0.0107558368367201,-1.19640181653194,
0.205233592872363));
#11561=CARTESIAN_POINT('Ctrl Pts',(-2.19605150036939E-16,-1.20714678905882,
1.11889664200504E-16));
#11562=CARTESIAN_POINT('Origin',(12.8681436286308,-1.83274446434879,0.6));
#11563=CARTESIAN_POINT('',(13.1677324890572,-1.83274446434879,0.615700786872883));
#11564=CARTESIAN_POINT('',(12.8354863574981,-2.13063349031027,0.613986809996789));
#11565=CARTESIAN_POINT('Origin',(12.8681436286308,-1.83274446434879,0.6));
#11566=CARTESIAN_POINT('',(12.8681436286308,-1.83274446434879,0.9));
#11567=CARTESIAN_POINT('Origin',(12.8681436286308,-1.83274446434879,0.6));
#11568=CARTESIAN_POINT('Origin',(12.8681436286308,-1.83274446434879,0.6));
#11569=CARTESIAN_POINT('Origin',(12.8681436286308,1.1,0.6));
#11570=CARTESIAN_POINT('',(13.1677324890572,1.1,0.615700786872883));
#11571=CARTESIAN_POINT('',(12.8681436286308,1.1,0.9));
#11572=CARTESIAN_POINT('Ctrl Pts',(12.8681436286308,-1.83274446434879,0.9));
#11573=CARTESIAN_POINT('Ctrl Pts',(11.0848390724976,-1.63724259846481,0.9));
#11574=CARTESIAN_POINT('Ctrl Pts',(6.90843812479705,-1.33014681916253,0.9));
#11575=CARTESIAN_POINT('Ctrl Pts',(2.72316671642812,-1.22963564084767,0.9));
#11576=CARTESIAN_POINT('Ctrl Pts',(0.331856371369203,-1.17491202960101,
0.9));
#11577=CARTESIAN_POINT('Ctrl Pts',(12.8586523934408,-1.91932043067563,0.9));
#11578=CARTESIAN_POINT('Ctrl Pts',(11.0774332085042,-1.7238803779394,0.89999435405169));
#11579=CARTESIAN_POINT('Ctrl Pts',(6.90489492800773,-1.41683381760594,0.900002805573959));
#11580=CARTESIAN_POINT('Ctrl Pts',(2.72111811994416,-1.31633797570969,0.90000078069347));
#11581=CARTESIAN_POINT('Ctrl Pts',(0.329872740993971,-1.26159263654569,
0.9));
#11582=CARTESIAN_POINT('Ctrl Pts',(12.8422006781022,-2.06938763738452,0.829321796184829));
#11583=CARTESIAN_POINT('Ctrl Pts',(11.0645720435655,-1.87407163985848,0.829602081442736));
#11584=CARTESIAN_POINT('Ctrl Pts',(6.89876476423634,-1.56711486110062,0.829953500700133));
#11585=CARTESIAN_POINT('Ctrl Pts',(2.71756729604702,-1.46664725828863,0.829952661937692));
#11586=CARTESIAN_POINT('Ctrl Pts',(0.326433810179884,-1.41186690836963,
0.829991693349937));
#11587=CARTESIAN_POINT('Ctrl Pts',(12.8358182377562,-2.12760618633201,0.679236780301187));
#11588=CARTESIAN_POINT('Ctrl Pts',(11.0595580661442,-1.93265366192027,0.679962478070753));
#11589=CARTESIAN_POINT('Ctrl Pts',(6.89634818471837,-1.62613750062048,0.680874066334139));
#11590=CARTESIAN_POINT('Ctrl Pts',(2.71617242066404,-1.52567909229178,0.680871998075852));
#11591=CARTESIAN_POINT('Ctrl Pts',(0.325082213976654,-1.47092890938704,
0.680973392412944));
#11592=CARTESIAN_POINT('Ctrl Pts',(12.8354863574981,-2.13063349031027,0.613986809996789));
#11593=CARTESIAN_POINT('Ctrl Pts',(11.0592740266891,-1.93586902238569,0.614841183901826));
#11594=CARTESIAN_POINT('Ctrl Pts',(6.89620783868867,-1.62958780289117,0.615922665333222));
#11595=CARTESIAN_POINT('Ctrl Pts',(2.71609101918193,-1.52912950204849,0.615919334096661));
#11596=CARTESIAN_POINT('Ctrl Pts',(0.325002675768742,-1.47440456706157,
0.616038917109795));
#11597=CARTESIAN_POINT('Ctrl Pts',(0.325002675768742,-1.47440456706157,
0.616038917109795));
#11598=CARTESIAN_POINT('Ctrl Pts',(2.71609101918193,-1.52912950204849,0.615919334096661));
#11599=CARTESIAN_POINT('Ctrl Pts',(6.89620783868867,-1.62958780289117,0.615922665333222));
#11600=CARTESIAN_POINT('Ctrl Pts',(11.0592740266891,-1.93586902238569,0.614841183901826));
#11601=CARTESIAN_POINT('Ctrl Pts',(12.8354863574981,-2.13063349031027,0.613986809996789));
#11602=CARTESIAN_POINT('Ctrl Pts',(12.8681436286308,-1.83274446434879,0.9));
#11603=CARTESIAN_POINT('Ctrl Pts',(11.0848390724976,-1.63724259846481,0.9));
#11604=CARTESIAN_POINT('Ctrl Pts',(6.90843812479705,-1.33014681916253,0.9));
#11605=CARTESIAN_POINT('Ctrl Pts',(2.72316671642812,-1.22963564084767,0.9));
#11606=CARTESIAN_POINT('Ctrl Pts',(0.331856371369203,-1.17491202960101,
0.9));
#11607=CARTESIAN_POINT('Ctrl Pts',(13.2003520234216,-1.86554403325358,-0.00671700702553119));
#11608=CARTESIAN_POINT('Ctrl Pts',(13.1894788444661,-1.85461114646479,0.200755606855839));
#11609=CARTESIAN_POINT('Ctrl Pts',(13.1786056663403,-1.84367795836273,0.40822820490283));
#11610=CARTESIAN_POINT('Ctrl Pts',(13.1677324890572,-1.83274446434879,0.615700786872884));
#11611=CARTESIAN_POINT('Ctrl Pts',(13.200220264666,-1.91338509859121,-0.00420290020003313));
#11612=CARTESIAN_POINT('Ctrl Pts',(13.1893470894366,-1.90245705934317,0.203270015787334));
#11613=CARTESIAN_POINT('Ctrl Pts',(13.1784738563058,-1.89152871992859,0.410742913234898));
#11614=CARTESIAN_POINT('Ctrl Pts',(13.1676006827814,-1.88060011874606,0.61821580043722));
#11615=CARTESIAN_POINT('Ctrl Pts',(13.1765676699515,-2.00888806967359,-0.000409897060868941));
#11616=CARTESIAN_POINT('Ctrl Pts',(13.1656896254949,-1.99796966505382,0.207063364242462));
#11617=CARTESIAN_POINT('Ctrl Pts',(13.1548115799789,-1.98705090404177,0.414536607525659));
#11618=CARTESIAN_POINT('Ctrl Pts',(13.1439334900924,-1.97613202744891,0.622009843787749));
#11619=CARTESIAN_POINT('Ctrl Pts',(13.0627995670833,-2.13884429305335,0.000475886042502645));
#11620=CARTESIAN_POINT('Ctrl Pts',(13.0518999280859,-2.12793157960824,0.207948441605934));
#11621=CARTESIAN_POINT('Ctrl Pts',(13.041000104914,-2.11701865581933,0.415420978499924));
#11622=CARTESIAN_POINT('Ctrl Pts',(13.0301002136907,-2.10610551685206,0.62289350259018));
#11623=CARTESIAN_POINT('Ctrl Pts',(12.9395973356642,-2.17103883395928,-0.00428435975826336));
#11624=CARTESIAN_POINT('Ctrl Pts',(12.9286794517625,-2.16011362679945,0.203186612960554));
#11625=CARTESIAN_POINT('Ctrl Pts',(12.9177614752639,-2.14918756369419,0.410657536673191));
#11626=CARTESIAN_POINT('Ctrl Pts',(12.9068431708026,-2.13826180183499,0.618128462699307));
#11627=CARTESIAN_POINT('Ctrl Pts',(12.8682582931239,-2.16344935299393,-0.00842301254802964));
#11628=CARTESIAN_POINT('Ctrl Pts',(12.857334548107,-2.15251107312608,0.1990469563258));
#11629=CARTESIAN_POINT('Ctrl Pts',(12.8464105706338,-2.1415724540018,0.406516897309109));
#11630=CARTESIAN_POINT('Ctrl Pts',(12.8354863574981,-2.13063349031027,0.61398680999679));
#11631=CARTESIAN_POINT('Ctrl Pts',(13.2,-1.86519007666192,-2.60208521396521E-17));
#11632=CARTESIAN_POINT('Ctrl Pts',(13.1892441622028,-1.85437516893481,0.20523361119958));
#11633=CARTESIAN_POINT('Ctrl Pts',(13.1784883252177,-1.84355996631422,0.410467206902138));
#11634=CARTESIAN_POINT('Ctrl Pts',(13.1677324890572,-1.83274446434879,0.615700786872884));
#11635=CARTESIAN_POINT('Ctrl Pts',(12.8354863574981,-2.13063349031027,0.61398680999679));
#11636=CARTESIAN_POINT('Ctrl Pts',(12.8462627343229,-2.14142441807303,0.409324567403199));
#11637=CARTESIAN_POINT('Ctrl Pts',(12.8570388818204,-2.15221501053143,0.204662297274642));
#11638=CARTESIAN_POINT('Ctrl Pts',(12.8678148030684,-2.16300527278357,2.15973072759112E-16));
#11639=CARTESIAN_POINT('Ctrl Pts',(12.868249917342,2.16344096606744,-0.0082639349430893));
#11640=CARTESIAN_POINT('Ctrl Pts',(12.8573289641336,2.15250548166836,0.19915300804817));
#11641=CARTESIAN_POINT('Ctrl Pts',(12.8464077785869,2.14156965818488,0.406569923163064));
#11642=CARTESIAN_POINT('Ctrl Pts',(12.8354863574981,2.13063349031027,0.613986809996789));
#11643=CARTESIAN_POINT('Ctrl Pts',(12.9158092820513,2.16850062662823,-0.00550483257449158));
#11644=CARTESIAN_POINT('Ctrl Pts',(12.9048922561706,2.15757374897544,0.201912774743134));
#11645=CARTESIAN_POINT('Ctrl Pts',(12.8939750281693,2.14664650750606,0.409330354360154));
#11646=CARTESIAN_POINT('Ctrl Pts',(12.8830575663678,2.13571903132675,0.616747911798467));
#11647=CARTESIAN_POINT('Ctrl Pts',(13.0132876381743,2.15534286385676,-0.00108956416640176));
#11648=CARTESIAN_POINT('Ctrl Pts',(13.002382910411,2.14442874534411,0.206329347217122));
#11649=CARTESIAN_POINT('Ctrl Pts',(12.9914779109393,2.13351435475356,0.413748232116966));
#11650=CARTESIAN_POINT('Ctrl Pts',(12.9805728576194,2.12259976690609,0.621167106093357));
#11651=CARTESIAN_POINT('Ctrl Pts',(13.1547834649542,2.05631410774027,0.001107541479323));
#11652=CARTESIAN_POINT('Ctrl Pts',(13.1439034803964,2.04540309863889,0.208527817346591));
#11653=CARTESIAN_POINT('Ctrl Pts',(13.1330234810862,2.03449182132921,0.415948079627069));
#11654=CARTESIAN_POINT('Ctrl Pts',(13.1221434051731,2.0235803832085,0.623368331037722));
#11655=CARTESIAN_POINT('Ctrl Pts',(13.2001460482598,1.93729725403583,-0.00278676680844524));
#11656=CARTESIAN_POINT('Ctrl Pts',(13.1892758011844,1.92637447722781,0.204633283810596));
#11657=CARTESIAN_POINT('Ctrl Pts',(13.1784050234814,1.91545126126866,0.412053283701094));
#11658=CARTESIAN_POINT('Ctrl Pts',(13.1675347796435,1.9045279459447,0.619473307219386));
#11659=CARTESIAN_POINT('Ctrl Pts',(13.2003436864113,1.86553565046225,-0.00655792739252892));
#11660=CARTESIAN_POINT('Ctrl Pts',(13.1894732864596,1.85460555778322,0.200861659936414));
#11661=CARTESIAN_POINT('Ctrl Pts',(13.1786028873373,1.84367516394377,0.408281231439009));
#11662=CARTESIAN_POINT('Ctrl Pts',(13.1677324890572,1.83274446434879,0.615700786872883));
#11663=CARTESIAN_POINT('Ctrl Pts',(12.8678148030684,2.16300527278357,-3.77302356024956E-17));
#11664=CARTESIAN_POINT('Ctrl Pts',(12.8570388818204,2.15221501053142,0.204662297274639));
#11665=CARTESIAN_POINT('Ctrl Pts',(12.8462627343229,2.14142441807303,0.409324567403198));
#11666=CARTESIAN_POINT('Ctrl Pts',(12.8354863574981,2.13063349031027,0.613986809996789));
#11667=CARTESIAN_POINT('Ctrl Pts',(13.1677324890572,1.83274446434879,0.615700786872883));
#11668=CARTESIAN_POINT('Ctrl Pts',(13.1784883252177,1.84355996631422,0.410467206902138));
#11669=CARTESIAN_POINT('Ctrl Pts',(13.1892441622028,1.85437516893481,0.20523361119958));
#11670=CARTESIAN_POINT('Ctrl Pts',(13.2,1.86519007666192,9.4542429440736E-17));
#11671=CARTESIAN_POINT('Ctrl Pts',(0.3318563713692,1.17491202960101,0.9));
#11672=CARTESIAN_POINT('Ctrl Pts',(2.72316671642811,1.22963564084767,0.9));
#11673=CARTESIAN_POINT('Ctrl Pts',(6.90843812479704,1.33014681916253,0.9));
#11674=CARTESIAN_POINT('Ctrl Pts',(11.0848390724976,1.63724259846481,0.9));
#11675=CARTESIAN_POINT('Ctrl Pts',(12.8681436286308,1.83274446434879,0.9));
#11676=CARTESIAN_POINT('Ctrl Pts',(0.329872740993969,1.26159263654569,0.9));
#11677=CARTESIAN_POINT('Ctrl Pts',(2.72111811994415,1.31633797570969,0.90000078069347));
#11678=CARTESIAN_POINT('Ctrl Pts',(6.90489492800774,1.41683381760594,0.90000280557396));
#11679=CARTESIAN_POINT('Ctrl Pts',(11.0774332085042,1.7238803779394,0.89999435405169));
#11680=CARTESIAN_POINT('Ctrl Pts',(12.8586523934408,1.91932043067563,0.9));
#11681=CARTESIAN_POINT('Ctrl Pts',(0.326433810179882,1.41186690836963,0.829991693349937));
#11682=CARTESIAN_POINT('Ctrl Pts',(2.71756729604703,1.46664725828863,0.829952661937692));
#11683=CARTESIAN_POINT('Ctrl Pts',(6.89876476423633,1.56711486110062,0.829953500700133));
#11684=CARTESIAN_POINT('Ctrl Pts',(11.0645720435655,1.87407163985848,0.829602081442736));
#11685=CARTESIAN_POINT('Ctrl Pts',(12.8422006781022,2.06938763738452,0.829321796184828));
#11686=CARTESIAN_POINT('Ctrl Pts',(0.325082213976652,1.47092890938703,0.680973392412944));
#11687=CARTESIAN_POINT('Ctrl Pts',(2.71617242066403,1.52567909229178,0.680871998075852));
#11688=CARTESIAN_POINT('Ctrl Pts',(6.89634818471838,1.62613750062048,0.680874066334139));
#11689=CARTESIAN_POINT('Ctrl Pts',(11.0595580661442,1.93265366192027,0.679962478070753));
#11690=CARTESIAN_POINT('Ctrl Pts',(12.8358182377562,2.12760618633201,0.679236780301187));
#11691=CARTESIAN_POINT('Ctrl Pts',(0.32500267576874,1.47440456706157,0.616038917109795));
#11692=CARTESIAN_POINT('Ctrl Pts',(2.71609101918192,1.52912950204849,0.615919334096661));
#11693=CARTESIAN_POINT('Ctrl Pts',(6.89620783868868,1.62958780289117,0.615922665333222));
#11694=CARTESIAN_POINT('Ctrl Pts',(11.0592740266891,1.93586902238569,0.614841183901826));
#11695=CARTESIAN_POINT('Ctrl Pts',(12.8354863574981,2.13063349031027,0.613986809996789));
#11696=CARTESIAN_POINT('Ctrl Pts',(12.8354863574981,2.13063349031027,0.613986809996789));
#11697=CARTESIAN_POINT('Ctrl Pts',(11.0592740266891,1.93586902238569,0.614841183901826));
#11698=CARTESIAN_POINT('Ctrl Pts',(6.89620783868868,1.62958780289117,0.615922665333222));
#11699=CARTESIAN_POINT('Ctrl Pts',(2.71609101918192,1.52912950204849,0.615919334096661));
#11700=CARTESIAN_POINT('Ctrl Pts',(0.32500267576874,1.47440456706157,0.616038917109795));
#11701=CARTESIAN_POINT('Ctrl Pts',(0.331856371879031,1.17491202961268,0.900000000000001));
#11702=CARTESIAN_POINT('Ctrl Pts',(2.72316671676804,1.22963564085583,0.9));
#11703=CARTESIAN_POINT('Ctrl Pts',(6.90843812496665,1.330146819175,0.9));
#11704=CARTESIAN_POINT('Ctrl Pts',(11.0848390724976,1.63724259846481,0.9));
#11705=CARTESIAN_POINT('Ctrl Pts',(12.8681436286308,1.83274446434879,0.9));
#11706=CARTESIAN_POINT('Ctrl Pts',(-0.00034095850043725,1.20748740317979,
-0.0065058757516861));
#11707=CARTESIAN_POINT('Ctrl Pts',(0.0105285311667133,1.19662889149835,
0.200896342313063));
#11708=CARTESIAN_POINT('Ctrl Pts',(0.0213980209804115,1.18577043337405,
0.408298563174108));
#11709=CARTESIAN_POINT('Ctrl Pts',(0.0322675109428289,1.17491202960101,
0.615700786872884));
#11710=CARTESIAN_POINT('Ctrl Pts',(-9.96670524854573E-5,1.295669506487,
-0.00190176065173685));
#11711=CARTESIAN_POINT('Ctrl Pts',(0.0107698931059531,1.28480880908357,
0.205500324005663));
#11712=CARTESIAN_POINT('Ctrl Pts',(0.0216392211477595,1.27394827585187,
0.412902429485043));
#11713=CARTESIAN_POINT('Ctrl Pts',(0.0325087822871292,1.26308766450658,
0.62030451837231));
#11714=CARTESIAN_POINT('Ctrl Pts',(0.0728623575603101,1.44853010213391,
0.00227745497540766));
#11715=CARTESIAN_POINT('Ctrl Pts',(0.0837280751164453,1.43766588856392,
0.209679530627308));
#11716=CARTESIAN_POINT('Ctrl Pts',(0.0945938325013454,1.42680163888532,
0.41708160190494));
#11717=CARTESIAN_POINT('Ctrl Pts',(0.105459512942901,1.41593747613444,0.624483681552028));
#11718=CARTESIAN_POINT('Ctrl Pts',(0.226308920038025,1.50529438233544,-0.00279245331904538));
#11719=CARTESIAN_POINT('Ctrl Pts',(0.237168779176494,1.4944331215396,0.204610074087555));
#11720=CARTESIAN_POINT('Ctrl Pts',(0.248028678199983,1.48357195724705,0.412012604182119));
#11721=CARTESIAN_POINT('Ctrl Pts',(0.258888441593434,1.47271077595937,0.619415140009235));
#11722=CARTESIAN_POINT('Ctrl Pts',(0.292428177212438,1.50698080067503,-0.00616932457891824));
#11723=CARTESIAN_POINT('Ctrl Pts',(0.303286399461314,1.49612200437087,0.201233417384176));
#11724=CARTESIAN_POINT('Ctrl Pts',(0.314144565926839,1.48526325958177,0.408636164588429));
#11725=CARTESIAN_POINT('Ctrl Pts',(0.325002675768741,1.47440456706157,0.616038917109795));
#11726=CARTESIAN_POINT('Ctrl Pts',(1.62630325872826E-19,1.20714678905882,
-9.93129189996722E-17));
#11727=CARTESIAN_POINT('Ctrl Pts',(0.0107558368367203,1.19640181653194,
0.205233592872363));
#11728=CARTESIAN_POINT('Ctrl Pts',(0.0215116738169619,1.18565689645617,
0.410467188483274));
#11729=CARTESIAN_POINT('Ctrl Pts',(0.0322675109428289,1.17491202960101,
0.615700786872884));
#11730=CARTESIAN_POINT('Ctrl Pts',(0.325002675768741,1.47440456706157,0.616038917109795));
#11731=CARTESIAN_POINT('Ctrl Pts',(0.314252226354851,1.48515559337638,0.410692606218907));
#11732=CARTESIAN_POINT('Ctrl Pts',(0.30350172143464,1.49590667092872,0.205346300540215));
#11733=CARTESIAN_POINT('Ctrl Pts',(0.292751161823635,1.50665779898694,-1.27502175484295E-16));
#11734=CARTESIAN_POINT('Ctrl Pts',(12.8678148030684,-2.16300527278356,0.));
#11735=CARTESIAN_POINT('Ctrl Pts',(12.8575947095063,-2.15224352891768,0.205346305703265));
#11736=CARTESIAN_POINT('Ctrl Pts',(12.8473746159443,-2.14148178505179,0.41069261140653));
#11737=CARTESIAN_POINT('Ctrl Pts',(12.8371545223823,-2.13072004118591,0.616038917109795));
#11738=CARTESIAN_POINT('Ctrl Pts',(8.67612692265345,-1.70561506876628,0.));
#11739=CARTESIAN_POINT('Ctrl Pts',(8.67274165808153,-1.69485332490039,0.205346305703265));
#11740=CARTESIAN_POINT('Ctrl Pts',(8.66935639350961,-1.68409158103451,0.41069261140653));
#11741=CARTESIAN_POINT('Ctrl Pts',(8.6659711289377,-1.67332983716862,0.616038917109795));
#11742=CARTESIAN_POINT('Ctrl Pts',(4.48443904223854,-1.60211086545473,0.));
#11743=CARTESIAN_POINT('Ctrl Pts',(4.48788860665674,-1.59134912158884,0.205346305703265));
#11744=CARTESIAN_POINT('Ctrl Pts',(4.49133817107494,-1.58058737772296,0.41069261140653));
#11745=CARTESIAN_POINT('Ctrl Pts',(4.49478773549313,-1.56982563385707,0.616038917109795));
#11746=CARTESIAN_POINT('Ctrl Pts',(0.292751161823634,-1.50665779898694,
0.));
#11747=CARTESIAN_POINT('Ctrl Pts',(0.303035555231945,-1.49589605512106,
0.205346305703265));
#11748=CARTESIAN_POINT('Ctrl Pts',(0.313319948640256,-1.48513431125517,
0.41069261140653));
#11749=CARTESIAN_POINT('Ctrl Pts',(0.323604342048567,-1.47437256738929,
0.616038917109795));
#11750=CARTESIAN_POINT('Origin',(0.,-1.5,0.));
#11751=CARTESIAN_POINT('Origin',(6.87409734069396,-2.22044604925031E-16,
0.9));
#11752=CARTESIAN_POINT('Ctrl Pts',(0.292751161823634,1.50665779898694,0.));
#11753=CARTESIAN_POINT('Ctrl Pts',(0.303035555231945,1.49589605512106,0.205346305703265));
#11754=CARTESIAN_POINT('Ctrl Pts',(0.313319948640256,1.48513431125517,0.41069261140653));
#11755=CARTESIAN_POINT('Ctrl Pts',(0.323604342048567,1.47437256738929,0.616038917109795));
#11756=CARTESIAN_POINT('Ctrl Pts',(4.48443904223854,1.60211086545473,0.));
#11757=CARTESIAN_POINT('Ctrl Pts',(4.48788860665674,1.59134912158884,0.205346305703265));
#11758=CARTESIAN_POINT('Ctrl Pts',(4.49133817107493,1.58058737772296,0.41069261140653));
#11759=CARTESIAN_POINT('Ctrl Pts',(4.49478773549313,1.56982563385707,0.616038917109795));
#11760=CARTESIAN_POINT('Ctrl Pts',(8.67612692265345,1.70561506876628,0.));
#11761=CARTESIAN_POINT('Ctrl Pts',(8.67274165808153,1.69485332490039,0.205346305703265));
#11762=CARTESIAN_POINT('Ctrl Pts',(8.66935639350961,1.68409158103451,0.41069261140653));
#11763=CARTESIAN_POINT('Ctrl Pts',(8.66597112893769,1.67332983716862,0.616038917109795));
#11764=CARTESIAN_POINT('Ctrl Pts',(12.8678148030684,2.16300527278356,0.));
#11765=CARTESIAN_POINT('Ctrl Pts',(12.8575947095063,2.15224352891768,0.205346305703265));
#11766=CARTESIAN_POINT('Ctrl Pts',(12.8473746159443,2.14148178505179,0.41069261140653));
#11767=CARTESIAN_POINT('Ctrl Pts',(12.8371545223823,2.13072004118591,0.616038917109795));
#11768=CARTESIAN_POINT('Origin',(13.2,2.2,0.));
#11769=CARTESIAN_POINT('',(0.,0.,0.));
#11770=CARTESIAN_POINT('Origin',(6.87409734069396,-2.22251806091942E-16,
0.7));
#11771=CARTESIAN_POINT('',(3.31825992066485,1.2493322588334,0.7));
#11772=CARTESIAN_POINT('',(4.3,1.27917501057225,0.7));
#11773=CARTESIAN_POINT('Ctrl Pts',(3.31826243508713,1.24933270901874,0.7));
#11774=CARTESIAN_POINT('Ctrl Pts',(3.64552542112514,1.25866821321074,0.7));
#11775=CARTESIAN_POINT('Ctrl Pts',(3.97277304530853,1.26856018917077,0.7));
#11776=CARTESIAN_POINT('Ctrl Pts',(4.30000000005992,1.27917501058303,0.7));
#11777=CARTESIAN_POINT('',(4.3,-1.27917501057184,0.7));
#11778=CARTESIAN_POINT('',(4.3,0.742407407407408,0.7));
#11779=CARTESIAN_POINT('',(3.31825992075695,-1.24933225883136,0.7));
#11780=CARTESIAN_POINT('Ctrl Pts',(4.3000000000599,-1.27917501058303,0.7));
#11781=CARTESIAN_POINT('Ctrl Pts',(3.97277304533917,-1.26856018917177,0.7));
#11782=CARTESIAN_POINT('Ctrl Pts',(3.64552542118644,-1.25866821321259,0.7));
#11783=CARTESIAN_POINT('Ctrl Pts',(3.3182624351791,-1.24933270902137,0.7));
#11784=CARTESIAN_POINT('',(3.26759951430388,-1.24789152572578,0.7));
#11785=CARTESIAN_POINT('Ctrl Pts',(3.26760216044043,-1.24789199949781,0.7));
#11786=CARTESIAN_POINT('Ctrl Pts',(3.27154046708102,-1.24840675231115,0.699999999449966));
#11787=CARTESIAN_POINT('Ctrl Pts',(3.27549053112987,-1.2488275353013,0.699997549264952));
#11788=CARTESIAN_POINT('Ctrl Pts',(3.27944900419773,-1.24915404112413,0.699995443099811));
#11789=CARTESIAN_POINT('Ctrl Pts',(3.28202272903949,-1.24936632907779,0.699994073710794));
#11790=CARTESIAN_POINT('Ctrl Pts',(3.28459959180148,-1.24953872742098,0.699992815093061));
#11791=CARTESIAN_POINT('Ctrl Pts',(3.28717866899733,-1.24967118132558,0.699992046536556));
#11792=CARTESIAN_POINT('Ctrl Pts',(3.28888409507617,-1.24975876704947,0.699991538325205));
#11793=CARTESIAN_POINT('Ctrl Pts',(3.29059037034979,-1.2498288805585,0.699991238158591));
#11794=CARTESIAN_POINT('Ctrl Pts',(3.29229723346923,-1.24988151179005,0.69999118215758));
#11795=CARTESIAN_POINT('Ctrl Pts',(3.29393274317941,-1.24993194283473,0.699991128497625));
#11796=CARTESIAN_POINT('Ctrl Pts',(3.29556870469678,-1.24996631998408,0.699991298652463));
#11797=CARTESIAN_POINT('Ctrl Pts',(3.29720488848534,-1.24998463806557,0.699991673963628));
#11798=CARTESIAN_POINT('Ctrl Pts',(3.29943508678369,-1.25000960650399,0.699992185531049));
#11799=CARTESIAN_POINT('Ctrl Pts',(3.30166551218918,-1.25000473681137,0.699993084765318));
#11800=CARTESIAN_POINT('Ctrl Pts',(3.30389557412726,-1.24997002667259,0.699994176731177));
#11801=CARTESIAN_POINT('Ctrl Pts',(3.30868977915254,-1.24989540653807,0.699996524248132));
#11802=CARTESIAN_POINT('Ctrl Pts',(3.31348068594496,-1.24968290539118,0.699999999312134));
#11803=CARTESIAN_POINT('Ctrl Pts',(3.3182624351791,-1.24933270902137,0.7));
#11804=CARTESIAN_POINT('',(1.1,-1.19266190204492,0.7));
#11805=CARTESIAN_POINT('Ctrl Pts',(3.26760216044045,-1.24789199949781,0.7));
#11806=CARTESIAN_POINT('Ctrl Pts',(2.54512260523322,-1.2274084473838,0.7));
#11807=CARTESIAN_POINT('Ctrl Pts',(1.82256951666701,-1.20959509718369,0.7));
#11808=CARTESIAN_POINT('Ctrl Pts',(1.09999999999999,-1.19266190204553,0.7));
#11809=CARTESIAN_POINT('',(1.1,1.19266190204492,0.7));
#11810=CARTESIAN_POINT('',(1.1,-0.696450594095222,0.7));
#11811=CARTESIAN_POINT('',(3.26759952419083,1.24789152650872,0.7));
#11812=CARTESIAN_POINT('Ctrl Pts',(1.09999999999999,1.19266190204553,0.7));
#11813=CARTESIAN_POINT('Ctrl Pts',(1.82256951996781,1.20959509726105,0.7));
#11814=CARTESIAN_POINT('Ctrl Pts',(2.54512261183467,1.22740844754655,0.7));
#11815=CARTESIAN_POINT('Ctrl Pts',(3.26760217034162,1.24789199977852,0.7));
#11816=CARTESIAN_POINT('Ctrl Pts',(3.3182624351791,1.24933270902137,0.7));
#11817=CARTESIAN_POINT('Ctrl Pts',(3.3143012451848,1.2496228108833,0.699999999430174));
#11818=CARTESIAN_POINT('Ctrl Pts',(3.31033365565543,1.24981842655856,0.699997549220164));
#11819=CARTESIAN_POINT('Ctrl Pts',(3.30636302717881,1.24991943948955,0.699995443052606));
#11820=CARTESIAN_POINT('Ctrl Pts',(3.30378139908369,1.24998511620097,0.699994073661998));
#11821=CARTESIAN_POINT('Ctrl Pts',(3.3011989045204,1.25001078941611,0.699992815050698));
#11822=CARTESIAN_POINT('Ctrl Pts',(3.29861646861803,1.2499964568765,0.699992046505716));
#11823=CARTESIAN_POINT('Ctrl Pts',(3.2969088217217,1.24998697942277,0.699991538302026));
#11824=CARTESIAN_POINT('Ctrl Pts',(3.29520131971864,1.24996000972381,0.699991238145114));
#11825=CARTESIAN_POINT('Ctrl Pts',(3.29349422410899,1.24991555258537,0.699991182154076));
#11826=CARTESIAN_POINT('Ctrl Pts',(3.29185849176351,1.24987295392896,0.699991128503682));
#11827=CARTESIAN_POINT('Ctrl Pts',(3.29022322047391,1.2498143016413,0.699991298668259));
#11828=CARTESIAN_POINT('Ctrl Pts',(3.28858863969825,1.2497396036024,0.699991673987721));
#11829=CARTESIAN_POINT('Ctrl Pts',(3.286360626573,1.24963778654105,0.699992185566407));
#11830=CARTESIAN_POINT('Ctrl Pts',(3.28413408201674,1.24950616665997,0.699993084809042));
#11831=CARTESIAN_POINT('Ctrl Pts',(3.2819095957713,1.24934477520901,0.699994176777649));
#11832=CARTESIAN_POINT('Ctrl Pts',(3.27712738077041,1.24899781481787,0.699996524298861));
#11833=CARTESIAN_POINT('Ctrl Pts',(3.27235629258357,1.24851338385513,0.699999999330822));
#11834=CARTESIAN_POINT('Ctrl Pts',(3.26760217026193,1.24789200078152,0.699999999999999));
#11835=CARTESIAN_POINT('',(3.15,1.,0.7));
#11836=CARTESIAN_POINT('Origin',(3.3,1.,0.7));
#11837=CARTESIAN_POINT('',(3.15,-1.,0.7));
#11838=CARTESIAN_POINT('Origin',(3.3,-1.,0.7));
#11839=CARTESIAN_POINT('',(1.6,-4.89858719658941E-17,0.7));
#11840=CARTESIAN_POINT('Origin',(2.,0.,0.7));
#11841=CARTESIAN_POINT('Origin',(9.9,-1.,0.8));
#11842=CARTESIAN_POINT('',(9.75,-1.,0.9));
#11843=CARTESIAN_POINT('Origin',(9.9,-1.,0.9));
#11844=CARTESIAN_POINT('',(9.75,-1.,0.7));
#11845=CARTESIAN_POINT('',(9.75,-1.,0.8));
#11846=CARTESIAN_POINT('Origin',(9.9,-1.,0.7));
#11847=CARTESIAN_POINT('Origin',(3.3,-1.,0.8));
#11848=CARTESIAN_POINT('',(3.15,-1.,0.9));
#11849=CARTESIAN_POINT('Origin',(3.3,-1.,0.9));
#11850=CARTESIAN_POINT('',(3.15,-1.,0.8));
#11851=CARTESIAN_POINT('Origin',(3.3,1.,0.8));
#11852=CARTESIAN_POINT('',(3.15,1.,0.9));
#11853=CARTESIAN_POINT('Origin',(3.3,1.,0.9));
#11854=CARTESIAN_POINT('',(3.15,1.,0.8));
#11855=CARTESIAN_POINT('Origin',(9.9,1.,0.8));
#11856=CARTESIAN_POINT('',(9.75,1.,0.9));
#11857=CARTESIAN_POINT('Origin',(9.9,1.,0.9));
#11858=CARTESIAN_POINT('',(9.75,1.,0.7));
#11859=CARTESIAN_POINT('',(9.75,1.,0.8));
#11860=CARTESIAN_POINT('Origin',(9.9,1.,0.7));
#11861=CARTESIAN_POINT('Origin',(11.3732050807569,0.3,0.9));
#11862=CARTESIAN_POINT('',(11.3732050807569,0.3,0.9));
#11863=CARTESIAN_POINT('',(11.5464101615138,0.,0.9));
#11864=CARTESIAN_POINT('',(10.8757685185329,1.16158539931442,0.9));
#11865=CARTESIAN_POINT('',(11.3732050807569,0.3,0.6));
#11866=CARTESIAN_POINT('',(11.3732050807569,0.3,0.9));
#11867=CARTESIAN_POINT('',(11.5464101615138,0.,0.6));
#11868=CARTESIAN_POINT('',(11.5464101615138,0.,0.6));
#11869=CARTESIAN_POINT('',(11.5464101615138,0.,0.9));
#11870=CARTESIAN_POINT('Origin',(11.0267949192431,0.3,0.9));
#11871=CARTESIAN_POINT('',(11.0267949192431,0.3,0.9));
#11872=CARTESIAN_POINT('',(8.95044612996854,0.3,0.9));
#11873=CARTESIAN_POINT('',(11.0267949192431,0.3,0.6));
#11874=CARTESIAN_POINT('',(11.0267949192431,0.3,0.9));
#11875=CARTESIAN_POINT('',(11.3732050807569,0.3,0.6));
#11876=CARTESIAN_POINT('Origin',(10.8535898384862,5.55111512312578E-17,
0.9));
#11877=CARTESIAN_POINT('',(10.8535898384862,4.24230095489963E-17,0.9));
#11878=CARTESIAN_POINT('',(10.3561532762622,-0.86158539931442,0.9));
#11879=CARTESIAN_POINT('',(10.8535898384862,5.55111512312578E-17,0.6));
#11880=CARTESIAN_POINT('',(10.8535898384862,4.24230095489963E-17,0.9));
#11881=CARTESIAN_POINT('',(11.0267949192431,0.3,0.6));
#11882=CARTESIAN_POINT('Origin',(11.0267949192431,-0.3,0.9));
#11883=CARTESIAN_POINT('',(11.0267949192431,-0.3,0.9));
#11884=CARTESIAN_POINT('',(10.4427558166406,0.71158539931442,0.9));
#11885=CARTESIAN_POINT('',(11.0267949192431,-0.3,0.6));
#11886=CARTESIAN_POINT('',(11.0267949192431,-0.3,0.9));
#11887=CARTESIAN_POINT('',(10.8535898384862,4.24230095489963E-17,0.6));
#11888=CARTESIAN_POINT('Origin',(11.3732050807569,-0.3,0.9));
#11889=CARTESIAN_POINT('',(11.3732050807569,-0.3,0.9));
#11890=CARTESIAN_POINT('',(9.12365121072543,-0.3,0.9));
#11891=CARTESIAN_POINT('',(11.3732050807569,-0.3,0.6));
#11892=CARTESIAN_POINT('',(11.3732050807569,-0.3,0.9));
#11893=CARTESIAN_POINT('',(11.0267949192431,-0.3,0.6));
#11894=CARTESIAN_POINT('Origin',(11.5464101615138,0.,0.9));
#11895=CARTESIAN_POINT('',(10.9623710589113,-1.01158539931442,0.9));
#11896=CARTESIAN_POINT('',(11.3732050807569,-0.3,0.6));
#11897=CARTESIAN_POINT('Origin',(11.2,5.55111512312578E-17,0.6));
#11898=CARTESIAN_POINT('',(11.03,-2.0818995585505E-17,0.6));
#11899=CARTESIAN_POINT('Origin',(11.2,0.,0.6));
#11900=CARTESIAN_POINT('Origin',(2.17320508075689,0.3,0.9));
#11901=CARTESIAN_POINT('',(2.17320508075689,0.3,0.9));
#11902=CARTESIAN_POINT('',(2.34641016151378,0.,0.9));
#11903=CARTESIAN_POINT('',(2.82576851853285,-0.830273029389787,0.9));
#11904=CARTESIAN_POINT('',(2.17320508075689,0.3,0.6));
#11905=CARTESIAN_POINT('',(2.17320508075689,0.3,0.9));
#11906=CARTESIAN_POINT('',(2.34641016151378,0.,0.6));
#11907=CARTESIAN_POINT('',(2.34641016151378,0.,0.6));
#11908=CARTESIAN_POINT('',(2.34641016151378,0.,0.9));
#11909=CARTESIAN_POINT('Origin',(1.82679491924311,0.3,0.9));
#11910=CARTESIAN_POINT('',(1.82679491924311,0.3,0.9));
#11911=CARTESIAN_POINT('',(4.35044612996854,0.3,0.9));
#11912=CARTESIAN_POINT('',(1.82679491924311,0.3,0.6));
#11913=CARTESIAN_POINT('',(1.82679491924311,0.3,0.9));
#11914=CARTESIAN_POINT('',(2.17320508075689,0.3,0.6));
#11915=CARTESIAN_POINT('Origin',(1.65358983848622,5.55111512312578E-17,
0.9));
#11916=CARTESIAN_POINT('',(1.65358983848622,4.24230095489963E-17,0.9));
#11917=CARTESIAN_POINT('',(2.30615327626219,1.13027302938979,0.9));
#11918=CARTESIAN_POINT('',(1.65358983848622,5.55111512312578E-17,0.6));
#11919=CARTESIAN_POINT('',(1.65358983848622,4.24230095489963E-17,0.9));
#11920=CARTESIAN_POINT('',(1.82679491924311,0.3,0.6));
#11921=CARTESIAN_POINT('Origin',(1.82679491924311,-0.3,0.9));
#11922=CARTESIAN_POINT('',(1.82679491924311,-0.3,0.9));
#11923=CARTESIAN_POINT('',(2.39275581664063,-1.28027302938979,0.9));
#11924=CARTESIAN_POINT('',(1.82679491924311,-0.3,0.6));
#11925=CARTESIAN_POINT('',(1.82679491924311,-0.3,0.9));
#11926=CARTESIAN_POINT('',(1.65358983848622,4.24230095489963E-17,0.6));
#11927=CARTESIAN_POINT('Origin',(2.17320508075689,-0.3,0.9));
#11928=CARTESIAN_POINT('',(2.17320508075689,-0.3,0.9));
#11929=CARTESIAN_POINT('',(4.52365121072543,-0.3,0.9));
#11930=CARTESIAN_POINT('',(2.17320508075689,-0.3,0.6));
#11931=CARTESIAN_POINT('',(2.17320508075689,-0.3,0.9));
#11932=CARTESIAN_POINT('',(1.82679491924311,-0.3,0.6));
#11933=CARTESIAN_POINT('Origin',(2.34641016151378,0.,0.9));
#11934=CARTESIAN_POINT('',(2.9123710589113,0.980273029389787,0.9));
#11935=CARTESIAN_POINT('',(2.17320508075689,-0.3,0.6));
#11936=CARTESIAN_POINT('Origin',(2.,5.55111512312578E-17,0.6));
#11937=CARTESIAN_POINT('',(1.83,-2.0818995585505E-17,0.6));
#11938=CARTESIAN_POINT('Origin',(2.,0.,0.6));
#11939=CARTESIAN_POINT('Origin',(2.,0.,0.45));
#11940=CARTESIAN_POINT('',(1.83,-2.0818995585505E-17,0.32));
#11941=CARTESIAN_POINT('',(1.83,2.0818995585505E-17,0.45));
#11942=CARTESIAN_POINT('Origin',(2.,0.,0.32));
#11943=CARTESIAN_POINT('Origin',(11.2,0.,0.45));
#11944=CARTESIAN_POINT('',(11.03,-2.0818995585505E-17,0.32));
#11945=CARTESIAN_POINT('',(11.03,2.0818995585505E-17,0.45));
#11946=CARTESIAN_POINT('Origin',(11.2,0.,0.32));
#11947=CARTESIAN_POINT('Origin',(12.4,-0.72,0.32));
#11948=CARTESIAN_POINT('',(0.200274469199584,-0.72,0.));
#11949=CARTESIAN_POINT('',(0.217044958570157,-0.72,0.32));
#11950=CARTESIAN_POINT('',(0.225070308370679,-0.72,0.473132796510599));
#11951=CARTESIAN_POINT('',(0.,-0.72,0.));
#11952=CARTESIAN_POINT('',(9.63649764092939,-0.72,0.));
#11953=CARTESIAN_POINT('',(0.0167704893705732,-0.72,0.32));
#11954=CARTESIAN_POINT('',(0.0253444014197637,-0.72,0.483599987759188));
#11955=CARTESIAN_POINT('',(-0.1,-0.72,0.32));
#11956=CARTESIAN_POINT('Origin',(12.4,-0.72,0.32));
#11957=CARTESIAN_POINT('',(0.9,-0.72,0.32));
#11958=CARTESIAN_POINT('',(0.9,-0.72,0.));
#11959=CARTESIAN_POINT('',(0.9,-0.72,0.16));
#11960=CARTESIAN_POINT('',(1.1,-0.72,0.32));
#11961=CARTESIAN_POINT('',(-0.1,-0.72,0.32));
#11962=CARTESIAN_POINT('',(1.1,-0.72,0.));
#11963=CARTESIAN_POINT('',(1.1,-0.72,0.16));
#11964=CARTESIAN_POINT('',(9.63649764092939,-0.72,0.));
#11965=CARTESIAN_POINT('Origin',(12.4,-0.72,0.32));
#11966=CARTESIAN_POINT('',(4.3,-0.72,0.32));
#11967=CARTESIAN_POINT('',(4.3,-0.72,0.));
#11968=CARTESIAN_POINT('',(4.3,-0.72,0.16));
#11969=CARTESIAN_POINT('',(4.5,-0.72,0.32));
#11970=CARTESIAN_POINT('',(-0.1,-0.72,0.32));
#11971=CARTESIAN_POINT('',(4.5,-0.72,0.));
#11972=CARTESIAN_POINT('',(4.5,-0.72,0.16));
#11973=CARTESIAN_POINT('',(9.63649764092939,-0.72,0.));
#11974=CARTESIAN_POINT('Origin',(12.4,-0.72,0.32));
#11975=CARTESIAN_POINT('',(8.7,-0.72,0.32));
#11976=CARTESIAN_POINT('',(8.7,-0.72,0.));
#11977=CARTESIAN_POINT('',(8.7,-0.72,0.16));
#11978=CARTESIAN_POINT('',(8.9,-0.72,0.32));
#11979=CARTESIAN_POINT('',(-0.1,-0.72,0.32));
#11980=CARTESIAN_POINT('',(8.9,-0.72,0.));
#11981=CARTESIAN_POINT('',(8.9,-0.72,0.16));
#11982=CARTESIAN_POINT('',(9.63649764092939,-0.72,0.));
#11983=CARTESIAN_POINT('Origin',(-0.0999999999999996,0.72,0.32));
#11984=CARTESIAN_POINT('',(0.217044958570158,0.72,0.32));
#11985=CARTESIAN_POINT('',(0.200274469199584,0.72,0.));
#11986=CARTESIAN_POINT('',(0.207951231396534,0.72,0.146481348799182));
#11987=CARTESIAN_POINT('',(0.0167704893705736,0.72,0.32));
#11988=CARTESIAN_POINT('',(12.4,0.72,0.32));
#11989=CARTESIAN_POINT('',(0.,0.72,0.));
#11990=CARTESIAN_POINT('',(0.00822532444561912,0.72,0.156948540047771));
#11991=CARTESIAN_POINT('',(3.38649764092939,0.72,0.));
#11992=CARTESIAN_POINT('Origin',(-0.0999999999999996,0.72,0.32));
#11993=CARTESIAN_POINT('',(0.9,0.72,0.));
#11994=CARTESIAN_POINT('',(0.9,0.72,0.32));
#11995=CARTESIAN_POINT('',(0.9,0.72,0.16));
#11996=CARTESIAN_POINT('',(1.1,0.72,0.));
#11997=CARTESIAN_POINT('',(3.38649764092939,0.72,0.));
#11998=CARTESIAN_POINT('',(1.1,0.72,0.32));
#11999=CARTESIAN_POINT('',(1.1,0.72,0.16));
#12000=CARTESIAN_POINT('',(12.4,0.72,0.32));
#12001=CARTESIAN_POINT('Origin',(-0.0999999999999996,0.72,0.32));
#12002=CARTESIAN_POINT('',(4.3,0.72,0.));
#12003=CARTESIAN_POINT('',(4.3,0.72,0.32));
#12004=CARTESIAN_POINT('',(4.3,0.72,0.16));
#12005=CARTESIAN_POINT('',(4.5,0.72,0.));
#12006=CARTESIAN_POINT('',(3.38649764092939,0.72,0.));
#12007=CARTESIAN_POINT('',(4.5,0.72,0.32));
#12008=CARTESIAN_POINT('',(4.5,0.72,0.16));
#12009=CARTESIAN_POINT('',(12.4,0.72,0.32));
#12010=CARTESIAN_POINT('Origin',(6.15,0.,0.32));
#12011=CARTESIAN_POINT('',(1.6,-4.89858719658941E-17,0.32));
#12012=CARTESIAN_POINT('Origin',(2.,0.,0.32));
#12013=CARTESIAN_POINT('Origin',(6.15,0.,0.32));
#12014=CARTESIAN_POINT('',(10.8,-4.89858719658942E-17,0.32));
#12015=CARTESIAN_POINT('Origin',(11.2,0.,0.32));
#12016=CARTESIAN_POINT('Origin',(6.15,0.,0.32));
#12017=CARTESIAN_POINT('',(0.217044958570157,-0.75,0.32));
#12018=CARTESIAN_POINT('',(0.0167704893705736,-0.75,0.32));
#12019=CARTESIAN_POINT('Origin',(6.15,0.,0.32));
#12020=CARTESIAN_POINT('',(0.9,0.696450594095222,0.32));
#12021=CARTESIAN_POINT('',(1.1,-0.696450594095222,0.32));
#12022=CARTESIAN_POINT('Origin',(6.15,0.,0.32));
#12023=CARTESIAN_POINT('',(4.3,0.742407407407408,0.32));
#12024=CARTESIAN_POINT('',(4.5,-0.742407407407408,0.32));
#12025=CARTESIAN_POINT('Origin',(6.15,0.,0.32));
#12026=CARTESIAN_POINT('',(8.7,0.72,0.32));
#12027=CARTESIAN_POINT('',(8.7,0.844259259259259,0.32));
#12028=CARTESIAN_POINT('',(8.9,0.72,0.32));
#12029=CARTESIAN_POINT('',(12.4,0.72,0.32));
#12030=CARTESIAN_POINT('',(8.9,-0.844259259259259,0.32));
#12031=CARTESIAN_POINT('Origin',(-0.0999999999999996,0.72,0.32));
#12032=CARTESIAN_POINT('',(8.7,0.72,0.));
#12033=CARTESIAN_POINT('',(8.7,0.72,0.16));
#12034=CARTESIAN_POINT('',(8.9,0.72,0.));
#12035=CARTESIAN_POINT('',(3.38649764092939,0.72,0.));
#12036=CARTESIAN_POINT('',(8.9,0.72,0.16));
#12037=CARTESIAN_POINT('Origin',(12.4,1.99376954809806,0.));
#12038=CARTESIAN_POINT('',(12.4,1.91212902562343,0.));
#12039=CARTESIAN_POINT('',(12.4,-1.91212902562343,0.));
#12040=CARTESIAN_POINT('',(12.4,1.99376954809806,0.));
#12041=CARTESIAN_POINT('',(12.4,-1.8833055216247,0.604732563714112));
#12042=CARTESIAN_POINT('Ctrl Pts',(12.4,-1.8833055216247,0.604732563714112));
#12043=CARTESIAN_POINT('Ctrl Pts',(12.4,-1.88809880980762,0.504101072758768));
#12044=CARTESIAN_POINT('Ctrl Pts',(12.4,-1.89289370245628,0.403468941627095));
#12045=CARTESIAN_POINT('Ctrl Pts',(12.4,-1.90250151416087,0.201891903194028));
#12046=CARTESIAN_POINT('Ctrl Pts',(12.4,-1.90731451170285,0.100945553925438));
#12047=CARTESIAN_POINT('Ctrl Pts',(12.4,-1.91212902562343,0.));
#12048=CARTESIAN_POINT('',(12.4,-1.78288409287054,0.7));
#12049=CARTESIAN_POINT('Ctrl Pts',(12.4000000030461,-1.78288409409899,0.7));
#12050=CARTESIAN_POINT('Ctrl Pts',(12.4000000066823,-1.79082830277209,0.699999997040196));
#12051=CARTESIAN_POINT('Ctrl Pts',(12.4000021328137,-1.79871128857748,0.699006690321208));
#12052=CARTESIAN_POINT('Ctrl Pts',(12.4000039827682,-1.8063921320806,0.697119229445379));
#12053=CARTESIAN_POINT('Ctrl Pts',(12.4000049365067,-1.81035196808589,0.69614615460905));
#12054=CARTESIAN_POINT('Ctrl Pts',(12.4000058167808,-1.81425808325963,0.694934510320783));
#12055=CARTESIAN_POINT('Ctrl Pts',(12.400006432968,-1.81808986884151,0.693492707237305));
#12056=CARTESIAN_POINT('Ctrl Pts',(12.4000076352846,-1.82556652433459,0.690679432664999));
#12057=CARTESIAN_POINT('Ctrl Pts',(12.4000076271954,-1.83268048852469,0.687023315130674));
#12058=CARTESIAN_POINT('Ctrl Pts',(12.4000063864816,-1.83928589538344,0.682605693351404));
#12059=CARTESIAN_POINT('Ctrl Pts',(12.4000055969106,-1.84348947395919,0.679794387301037));
#12060=CARTESIAN_POINT('Ctrl Pts',(12.400004329084,-1.84748689691167,0.676673627174617));
#12061=CARTESIAN_POINT('Ctrl Pts',(12.4000032503406,-1.8512341074341,0.673255429390325));
#12062=CARTESIAN_POINT('Ctrl Pts',(12.4000023796213,-1.85425870830395,0.670496394655072));
#12063=CARTESIAN_POINT('Ctrl Pts',(12.4000016297172,-1.85710218072175,0.667559826261508));
#12064=CARTESIAN_POINT('Ctrl Pts',(12.4000016274617,-1.859744520612,0.664455546516084));
#12065=CARTESIAN_POINT('Ctrl Pts',(12.4000016230979,-1.86485672743849,0.658449612092435));
#12066=CARTESIAN_POINT('Ctrl Pts',(12.4000041080363,-1.86921906069885,0.651817317967817));
#12067=CARTESIAN_POINT('Ctrl Pts',(12.40000495371,-1.8727702927896,0.64472299566344));
#12068=CARTESIAN_POINT('Ctrl Pts',(12.4000050555652,-1.8731980125259,0.643868536819953));
#12069=CARTESIAN_POINT('Ctrl Pts',(12.4000051394069,-1.87361391018412,0.643007349425002));
#12070=CARTESIAN_POINT('Ctrl Pts',(12.4000052029357,-1.87401783114888,0.642139703315781));
#12071=CARTESIAN_POINT('Ctrl Pts',(12.4000057294153,-1.87736522853405,0.634949295858174));
#12072=CARTESIAN_POINT('Ctrl Pts',(12.4000043880804,-1.87985460663586,0.627401584261416));
#12073=CARTESIAN_POINT('Ctrl Pts',(12.4000025112034,-1.88143175301701,0.619663949188762));
#12074=CARTESIAN_POINT('Ctrl Pts',(12.4000013193515,-1.88243327046239,0.614750406220363));
#12075=CARTESIAN_POINT('Ctrl Pts',(12.4,-1.88306607129604,0.609759643802656));
#12076=CARTESIAN_POINT('Ctrl Pts',(12.4,-1.8833055216247,0.604732563714112));
#12077=CARTESIAN_POINT('',(12.4,1.78288409287164,0.7));
#12078=CARTESIAN_POINT('',(12.4,0.99688477404903,0.7));
#12079=CARTESIAN_POINT('',(12.4,1.8833055216247,0.604732563714112));
#12080=CARTESIAN_POINT('Ctrl Pts',(12.4,1.8833055216247,0.604732563714112));
#12081=CARTESIAN_POINT('Ctrl Pts',(12.4,1.88292893537322,0.612638709665068));
#12082=CARTESIAN_POINT('Ctrl Pts',(12.4000029905988,1.88158186833012,0.620459457162159));
#12083=CARTESIAN_POINT('Ctrl Pts',(12.400004351969,1.87934739482834,0.62803467841275));
#12084=CARTESIAN_POINT('Ctrl Pts',(12.4000050124983,1.87826324073514,0.631710133556493));
#12085=CARTESIAN_POINT('Ctrl Pts',(12.4000053733669,1.87696936339782,0.63532777623417));
#12086=CARTESIAN_POINT('Ctrl Pts',(12.4000053391329,1.87547104796815,0.638868146717817));
#12087=CARTESIAN_POINT('Ctrl Pts',(12.4000052683671,1.872373843052,0.646186534188034));
#12088=CARTESIAN_POINT('Ctrl Pts',(12.4000032465668,1.86844110215533,0.653093304890266));
#12089=CARTESIAN_POINT('Ctrl Pts',(12.4000021327941,1.86374151467895,0.659427433016556));
#12090=CARTESIAN_POINT('Ctrl Pts',(12.4000018304335,1.86246569800928,0.66114698527342));
#12091=CARTESIAN_POINT('Ctrl Pts',(12.4000016226794,1.86113309763036,0.662824214875179));
#12092=CARTESIAN_POINT('Ctrl Pts',(12.400001625255,1.85974452038344,0.664455546516227));
#12093=CARTESIAN_POINT('Ctrl Pts',(12.4000016287814,1.85784336180007,0.666689070188443));
#12094=CARTESIAN_POINT('Ctrl Pts',(12.400002024929,1.85583728779192,0.668836587948716));
#12095=CARTESIAN_POINT('Ctrl Pts',(12.4000025639666,1.85373364862045,0.670894373083513));
#12096=CARTESIAN_POINT('Ctrl Pts',(12.400004021536,1.84804536272624,0.676458668669153));
#12097=CARTESIAN_POINT('Ctrl Pts',(12.4000062945443,1.84171268252251,0.681305055194542));
#12098=CARTESIAN_POINT('Ctrl Pts',(12.4000070319583,1.83490078417639,0.685381489016216));
#12099=CARTESIAN_POINT('Ctrl Pts',(12.4000075068619,1.8305138392177,0.688006761722114));
#12100=CARTESIAN_POINT('Ctrl Pts',(12.4000074483741,1.82592714021755,0.69031203082117));
#12101=CARTESIAN_POINT('Ctrl Pts',(12.4000068708525,1.82117863971551,0.692273867243687));
#12102=CARTESIAN_POINT('Ctrl Pts',(12.4000059767178,1.81382688138917,0.695311236040001));
#12103=CARTESIAN_POINT('Ctrl Pts',(12.4000038254996,1.80617119073902,0.697493343451155));
#12104=CARTESIAN_POINT('Ctrl Pts',(12.4000020685374,1.7983596509798,0.698751345219246));
#12105=CARTESIAN_POINT('Ctrl Pts',(12.4000009204513,1.79325520389048,0.699573385900268));
#12106=CARTESIAN_POINT('Ctrl Pts',(12.400000005426,1.78808359082883,0.699999998062804));
#12107=CARTESIAN_POINT('Ctrl Pts',(12.4000000030461,1.78288409409899,0.7));
#12108=CARTESIAN_POINT('Ctrl Pts',(12.4,1.91212902562343,0.));
#12109=CARTESIAN_POINT('Ctrl Pts',(12.4,1.90731404243129,0.1009553931071));
#12110=CARTESIAN_POINT('Ctrl Pts',(12.4,1.9025005759122,0.201911581737034));
#12111=CARTESIAN_POINT('Ctrl Pts',(12.4,1.89289276481806,0.403488620176902));
#12112=CARTESIAN_POINT('Ctrl Pts',(12.4,1.88809834114759,0.504110911924693));
#12113=CARTESIAN_POINT('Ctrl Pts',(12.4,1.8833055216247,0.604732563714112));
#12114=CARTESIAN_POINT('Origin',(8.9,-1.68851851851852,0.));
#12115=CARTESIAN_POINT('',(8.9,1.62420669932031,0.));
#12116=CARTESIAN_POINT('',(8.9,-1.68851851851852,0.));
#12117=CARTESIAN_POINT('',(8.9,1.59320117118329,0.605106081470792));
#12118=CARTESIAN_POINT('Ctrl Pts',(8.9,1.59320117118329,0.605106081470792));
#12119=CARTESIAN_POINT('Ctrl Pts',(8.9,1.59837103562161,0.504197738990529));
#12120=CARTESIAN_POINT('Ctrl Pts',(8.9,1.60354126123154,0.403288838380538));
#12121=CARTESIAN_POINT('Ctrl Pts',(8.9,1.61387642009944,0.201587196710533));
#12122=CARTESIAN_POINT('Ctrl Pts',(8.9,1.61904141157348,0.100793304842659));
#12123=CARTESIAN_POINT('Ctrl Pts',(8.9,1.62420669932031,0.));
#12124=CARTESIAN_POINT('',(8.9,1.49312521822106,0.7));
#12125=CARTESIAN_POINT('Ctrl Pts',(8.9,1.49312521822106,0.7));
#12126=CARTESIAN_POINT('Ctrl Pts',(8.9,1.50104136823484,0.7));
#12127=CARTESIAN_POINT('Ctrl Pts',(8.90000131173634,1.50889623314995,0.699007530025307));
#12128=CARTESIAN_POINT('Ctrl Pts',(8.90000245364087,1.51654949575132,0.697121675771258));
#12129=CARTESIAN_POINT('Ctrl Pts',(8.9000030153269,1.52031402289636,0.696194051841344));
#12130=CARTESIAN_POINT('Ctrl Pts',(8.90000353645954,1.52402976767023,0.695049421358208));
#12131=CARTESIAN_POINT('Ctrl Pts',(8.90000391188735,1.52767894577544,0.693695149285802));
#12132=CARTESIAN_POINT('Ctrl Pts',(8.90000468147812,1.53515940869299,0.690919022244083));
#12133=CARTESIAN_POINT('Ctrl Pts',(8.90000470661952,1.54227958804117,0.687295426711095));
#12134=CARTESIAN_POINT('Ctrl Pts',(8.9000039635008,1.54889410374269,0.682907715777054));
#12135=CARTESIAN_POINT('Ctrl Pts',(8.90000349228854,1.55308837416723,0.680125464281631));
#12136=CARTESIAN_POINT('Ctrl Pts',(8.90000272405863,1.55707914411963,0.677034908766328));
#12137=CARTESIAN_POINT('Ctrl Pts',(8.90000205379677,1.56082314136721,0.673648333128258));
#12138=CARTESIAN_POINT('Ctrl Pts',(8.90000149471997,1.56394607304962,0.670823532879853));
#12139=CARTESIAN_POINT('Ctrl Pts',(8.90000100172653,1.56687805273397,0.667809941545923));
#12140=CARTESIAN_POINT('Ctrl Pts',(8.90000100003,1.56959740049228,0.664618488856983));
#12141=CARTESIAN_POINT('Ctrl Pts',(8.90000099684156,1.57470809805256,0.658620525035968));
#12142=CARTESIAN_POINT('Ctrl Pts',(8.90000253934467,1.57907071782202,0.651995745956818));
#12143=CARTESIAN_POINT('Ctrl Pts',(8.90000305932469,1.58262507990443,0.644909256877938));
#12144=CARTESIAN_POINT('Ctrl Pts',(8.90000311559331,1.58300970826793,0.644142406277414));
#12145=CARTESIAN_POINT('Ctrl Pts',(8.9000031627798,1.58338482682255,0.643370127200485));
#12146=CARTESIAN_POINT('Ctrl Pts',(8.90000319981124,1.58375032531468,0.642592615892991));
#12147=CARTESIAN_POINT('Ctrl Pts',(8.90000354178946,1.58712563340961,0.635412448897651));
#12148=CARTESIAN_POINT('Ctrl Pts',(8.90000272882427,1.58964525157545,0.627871187463612));
#12149=CARTESIAN_POINT('Ctrl Pts',(8.90000156924769,1.59125549206429,0.620136848214628));
#12150=CARTESIAN_POINT('Ctrl Pts',(8.90000082792478,1.59228492658837,0.615192247765769));
#12151=CARTESIAN_POINT('Ctrl Pts',(8.89999999997262,1.59294182914154,0.610168076493048));
#12152=CARTESIAN_POINT('Ctrl Pts',(8.9000000009702,1.5932011715731,0.605106081469384));
#12153=CARTESIAN_POINT('',(8.9,-1.49312521822001,0.7));
#12154=CARTESIAN_POINT('',(8.9,-0.844259259259259,0.7));
#12155=CARTESIAN_POINT('',(8.9,-1.59320117118329,0.605106081470792));
#12156=CARTESIAN_POINT('Ctrl Pts',(8.90000000097019,-1.5932011715731,0.605106081469384));
#12157=CARTESIAN_POINT('Ctrl Pts',(8.89999999941083,-1.59279578158415,0.613018716877257));
#12158=CARTESIAN_POINT('Ctrl Pts',(8.90000185372291,-1.59142151714118,0.620841302874248));
#12159=CARTESIAN_POINT('Ctrl Pts',(8.90000269095591,-1.58916270068609,0.628413601005994));
#12160=CARTESIAN_POINT('Ctrl Pts',(8.90000316003867,-1.58789713677684,0.632656188846207));
#12161=CARTESIAN_POINT('Ctrl Pts',(8.90000337414869,-1.58635289833986,0.636820251299613));
#12162=CARTESIAN_POINT('Ctrl Pts',(8.90000326408749,-1.58453800492682,0.640875626603871));
#12163=CARTESIAN_POINT('Ctrl Pts',(8.9000030675631,-1.58129734600662,0.648116871770122));
#12164=CARTESIAN_POINT('Ctrl Pts',(8.90000169351568,-1.5772322800227,0.654932667693845));
#12165=CARTESIAN_POINT('Ctrl Pts',(8.90000116172667,-1.57240747726376,0.66116027211862));
#12166=CARTESIAN_POINT('Ctrl Pts',(8.90000106146602,-1.57149783490479,0.662334391157823));
#12167=CARTESIAN_POINT('Ctrl Pts',(8.90000099955281,-1.57056105641498,0.663487533005214));
#12168=CARTESIAN_POINT('Ctrl Pts',(8.90000100072893,-1.56959740053727,0.664618488856962));
#12169=CARTESIAN_POINT('Ctrl Pts',(8.9000010030487,-1.56769671285427,0.666849154291726));
#12170=CARTESIAN_POINT('Ctrl Pts',(8.90000124864079,-1.56569149899762,0.668993559652069));
#12171=CARTESIAN_POINT('Ctrl Pts',(8.90000158179872,-1.56358911460694,0.671047966011734));
#12172=CARTESIAN_POINT('Ctrl Pts',(8.90000248280001,-1.55790336961918,0.676603957919834));
#12173=CARTESIAN_POINT('Ctrl Pts',(8.90000387848177,-1.55157399841983,0.681441805123218));
#12174=CARTESIAN_POINT('Ctrl Pts',(8.90000432886686,-1.54476515293017,0.68550782533293));
#12175=CARTESIAN_POINT('Ctrl Pts',(8.9000046162921,-1.54041990676133,0.688102664467623));
#12176=CARTESIAN_POINT('Ctrl Pts',(8.90000458123012,-1.53587841548674,0.69038248607508));
#12177=CARTESIAN_POINT('Ctrl Pts',(8.90000422571091,-1.53117752164703,0.692323975790708));
#12178=CARTESIAN_POINT('Ctrl Pts',(8.90000367147839,-1.52384911813356,0.695350638493274));
#12179=CARTESIAN_POINT('Ctrl Pts',(8.9000023358238,-1.51621796414731,0.697522741667433));
#12180=CARTESIAN_POINT('Ctrl Pts',(8.90000125519218,-1.50843132129101,0.698770821080692));
#12181=CARTESIAN_POINT('Ctrl Pts',(8.90000055451733,-1.5033825102871,0.699580068042664));
#12182=CARTESIAN_POINT('Ctrl Pts',(8.9,-1.49826772866746,0.7));
#12183=CARTESIAN_POINT('Ctrl Pts',(8.9,-1.49312521822106,0.7));
#12184=CARTESIAN_POINT('',(8.9,-1.62420669932031,0.));
#12185=CARTESIAN_POINT('Ctrl Pts',(8.9,-1.62420669932031,0.));
#12186=CARTESIAN_POINT('Ctrl Pts',(8.9,-1.61904139377919,0.100793652073202));
#12187=CARTESIAN_POINT('Ctrl Pts',(8.9,-1.61387638451174,0.201587891198165));
#12188=CARTESIAN_POINT('Ctrl Pts',(8.9,-1.60354122564866,0.403289532862703));
#12189=CARTESIAN_POINT('Ctrl Pts',(8.9,-1.59837101783099,0.50419808623799));
#12190=CARTESIAN_POINT('Ctrl Pts',(8.9,-1.59320117118329,0.605106081470792));
#12191=CARTESIAN_POINT('',(8.9,-1.68851851851852,0.));
#12192=CARTESIAN_POINT('Origin',(4.5,-1.48481481481482,0.));
#12193=CARTESIAN_POINT('',(4.5,1.41772989878425,0.));
#12194=CARTESIAN_POINT('',(4.5,-1.48481481481482,0.));
#12195=CARTESIAN_POINT('',(4.5,1.38566996325095,0.605286533624017));
#12196=CARTESIAN_POINT('Ctrl Pts',(4.5,1.38566996325095,0.605286533624017));
#12197=CARTESIAN_POINT('Ctrl Pts',(4.5,1.3910232158183,0.504222354021684));
#12198=CARTESIAN_POINT('Ctrl Pts',(4.5,1.39637635187357,0.403158168247774));
#12199=CARTESIAN_POINT('Ctrl Pts',(4.5,1.4070629957395,0.201395990303158));
#12200=CARTESIAN_POINT('Ctrl Pts',(4.5,1.41239650438775,0.100697998177668));
#12201=CARTESIAN_POINT('Ctrl Pts',(4.5,1.41772989878425,0.));
#12202=CARTESIAN_POINT('',(4.5,1.28575421950843,0.7));
#12203=CARTESIAN_POINT('Ctrl Pts',(4.5,1.28575421950843,0.7));
#12204=CARTESIAN_POINT('Ctrl Pts',(4.5,1.29366545802379,0.7));
#12205=CARTESIAN_POINT('Ctrl Pts',(4.50000067540813,1.30151306508378,0.699006020085879));
#12206=CARTESIAN_POINT('Ctrl Pts',(4.50000126278178,1.30915682219698,0.697118891599074));
#12207=CARTESIAN_POINT('Ctrl Pts',(4.50000159346398,1.31346013814185,0.696056467716811));
#12208=CARTESIAN_POINT('Ctrl Pts',(4.50000189442328,1.31769890045703,0.694709922559592));
#12209=CARTESIAN_POINT('Ctrl Pts',(4.50000208642664,1.32184639782974,0.693090275295953));
#12210=CARTESIAN_POINT('Ctrl Pts',(4.50000243009859,1.32927011415192,0.690191225399894));
#12211=CARTESIAN_POINT('Ctrl Pts',(4.50000235826664,1.33632110693134,0.686451804482762));
#12212=CARTESIAN_POINT('Ctrl Pts',(4.50000192249634,1.34285330390028,0.681953677325188));
#12213=CARTESIAN_POINT('Ctrl Pts',(4.5000016824508,1.3464515866709,0.679475868782656));
#12214=CARTESIAN_POINT('Ctrl Pts',(4.50000134086274,1.34989218134371,0.676766953538005));
#12215=CARTESIAN_POINT('Ctrl Pts',(4.50000103767597,1.35314674504257,0.67383503027087));
#12216=CARTESIAN_POINT('Ctrl Pts',(4.50000074242034,1.35631617169348,0.670979804009792));
#12217=CARTESIAN_POINT('Ctrl Pts',(4.50000047986374,1.35928994516467,0.667930335702103));
#12218=CARTESIAN_POINT('Ctrl Pts',(4.5000004798165,1.36204555935344,0.66469809744354));
#12219=CARTESIAN_POINT('Ctrl Pts',(4.5000004797289,1.36715559606013,0.658704204607119));
#12220=CARTESIAN_POINT('Ctrl Pts',(4.50000128456446,1.3715183542993,0.652083197653858));
#12221=CARTESIAN_POINT('Ctrl Pts',(4.50000155892095,1.37507421485048,0.645000595057188));
#12222=CARTESIAN_POINT('Ctrl Pts',(4.50000158702893,1.37543851484667,0.644274978272754));
#12223=CARTESIAN_POINT('Ctrl Pts',(4.50000161091379,1.37579430519483,0.643544496675346));
#12224=CARTESIAN_POINT('Ctrl Pts',(4.50000163009343,1.37614149316233,0.642809317076966));
#12225=CARTESIAN_POINT('Ctrl Pts',(4.50000181728783,1.37953006709248,0.635633923185928));
#12226=CARTESIAN_POINT('Ctrl Pts',(4.50000140772507,1.38206400387968,0.628095594687559));
#12227=CARTESIAN_POINT('Ctrl Pts',(4.50000081194859,1.38368993781387,0.620362729373495));
#12228=CARTESIAN_POINT('Ctrl Pts',(4.50000042990035,1.38473258588096,0.615403944208116));
#12229=CARTESIAN_POINT('Ctrl Pts',(4.49999999988018,1.38540098970406,0.610364492806037));
#12230=CARTESIAN_POINT('Ctrl Pts',(4.50000000014037,1.38566996330298,0.605286533623957));
#12231=CARTESIAN_POINT('',(4.5,-1.28575421950842,0.7));
#12232=CARTESIAN_POINT('',(4.5,-0.742407407407408,0.7));
#12233=CARTESIAN_POINT('',(4.5,-1.38566996325095,0.605286533624017));
#12234=CARTESIAN_POINT('Ctrl Pts',(4.50000000014037,-1.38566996330298,0.605286533623957));
#12235=CARTESIAN_POINT('Ctrl Pts',(4.49999999973491,-1.38525081272033,0.613199687771457));
#12236=CARTESIAN_POINT('Ctrl Pts',(4.50000095642016,-1.38386419754969,0.62102180968747));
#12237=CARTESIAN_POINT('Ctrl Pts',(4.50000138305812,-1.38159414679432,0.628592503408469));
#12238=CARTESIAN_POINT('Ctrl Pts',(4.50000162118259,-1.38032713666619,0.632818023740444));
#12239=CARTESIAN_POINT('Ctrl Pts',(4.50000172745986,-1.37878391728058,0.636965253716347));
#12240=CARTESIAN_POINT('Ctrl Pts',(4.50000166716583,-1.37697237493585,0.641004309729874));
#12241=CARTESIAN_POINT('Ctrl Pts',(4.50000155916287,-1.37372741146613,0.648239354085419));
#12242=CARTESIAN_POINT('Ctrl Pts',(4.50000084040372,-1.36965973349804,0.655049237033139));
#12243=CARTESIAN_POINT('Ctrl Pts',(4.50000056390271,-1.36483316768901,0.661270759279915));
#12244=CARTESIAN_POINT('Ctrl Pts',(4.50000051219424,-1.36393055121024,0.662434246679675));
#12245=CARTESIAN_POINT('Ctrl Pts',(4.50000048023544,-1.3630012658104,0.663577087492372));
#12246=CARTESIAN_POINT('Ctrl Pts',(4.50000048056391,-1.36204555937839,0.664698097443534));
#12247=CARTESIAN_POINT('Ctrl Pts',(4.50000048121673,-1.36014610273268,0.666926093123284));
#12248=CARTESIAN_POINT('Ctrl Pts',(4.50000060829837,-1.35814231322364,0.669067903674665));
#12249=CARTESIAN_POINT('Ctrl Pts',(4.50000078085101,-1.35604151212276,0.671119765431539));
#12250=CARTESIAN_POINT('Ctrl Pts',(4.50000124774248,-1.3503571825734,0.676671675324794));
#12251=CARTESIAN_POINT('Ctrl Pts',(4.50000197143062,-1.34402953514766,0.681505303070731));
#12252=CARTESIAN_POINT('Ctrl Pts',(4.50000220836427,-1.33722229030693,0.685566265232058));
#12253=CARTESIAN_POINT('Ctrl Pts',(4.50000235894787,-1.33289593407788,0.688147216755564));
#12254=CARTESIAN_POINT('Ctrl Pts',(4.50000234488938,-1.32837489877041,0.690415387400166));
#12255=CARTESIAN_POINT('Ctrl Pts',(4.50000216490635,-1.32369554581057,0.69234752884452));
#12256=CARTESIAN_POINT('Ctrl Pts',(4.50000188343739,-1.31637767466938,0.695369135087455));
#12257=CARTESIAN_POINT('Ctrl Pts',(4.50000119588393,-1.3087575932273,0.697536490026807));
#12258=CARTESIAN_POINT('Ctrl Pts',(4.50000064127173,-1.30098224657147,0.698779892333419));
#12259=CARTESIAN_POINT('Ctrl Pts',(4.50000028296845,-1.29595903898196,0.699583183579437));
#12260=CARTESIAN_POINT('Ctrl Pts',(4.5,-1.29087043558603,0.7));
#12261=CARTESIAN_POINT('Ctrl Pts',(4.5,-1.28575421950843,0.7));
#12262=CARTESIAN_POINT('',(4.5,-1.41772989878425,0.));
#12263=CARTESIAN_POINT('Ctrl Pts',(4.5,-1.41772989878425,0.));
#12264=CARTESIAN_POINT('Ctrl Pts',(4.5,-1.41239649634988,0.100698149937961));
#12265=CARTESIAN_POINT('Ctrl Pts',(4.5,-1.40706297966336,0.201396293824709));
#12266=CARTESIAN_POINT('Ctrl Pts',(4.5,-1.39637633579674,0.403158471769294));
#12267=CARTESIAN_POINT('Ctrl Pts',(4.5,-1.39102320777973,0.504222505781934));
#12268=CARTESIAN_POINT('Ctrl Pts',(4.5,-1.38566996325095,0.605286533624017));
#12269=CARTESIAN_POINT('',(4.5,-1.48481481481482,0.));
#12270=CARTESIAN_POINT('Origin',(1.1,-1.39290118819044,0.));
#12271=CARTESIAN_POINT('',(1.1,1.324891758307,0.));
#12272=CARTESIAN_POINT('',(1.1,-1.39290118819044,0.));
#12273=CARTESIAN_POINT('',(1.10000000295569,1.29254692766489,0.605334652628491));
#12274=CARTESIAN_POINT('Ctrl Pts',(1.10000000295569,1.29254692766489,0.605334652628491));
#12275=CARTESIAN_POINT('Ctrl Pts',(1.10000000295569,1.29794978210809,0.504228164786351));
#12276=CARTESIAN_POINT('Ctrl Pts',(1.1,1.30335245345465,0.403121008362245));
#12277=CARTESIAN_POINT('Ctrl Pts',(1.1,1.31413403739463,0.20134322693425));
#12278=CARTESIAN_POINT('Ctrl Pts',(1.1,1.31951302132877,0.100671299071668));
#12279=CARTESIAN_POINT('Ctrl Pts',(1.1,1.324891758307,0.));
#12280=CARTESIAN_POINT('Ctrl Pts',(1.1,1.19266190204553,0.7));
#12281=CARTESIAN_POINT('Ctrl Pts',(1.1,1.20057109129252,0.7));
#12282=CARTESIAN_POINT('Ctrl Pts',(1.10000046829629,1.20841685974333,0.699006220526237));
#12283=CARTESIAN_POINT('Ctrl Pts',(1.10000087277688,1.21605887983377,0.697119382842322));
#12284=CARTESIAN_POINT('Ctrl Pts',(1.10000109992184,1.22035042410288,0.696059787689036));
#12285=CARTESIAN_POINT('Ctrl Pts',(1.10000130563842,1.22457776983048,0.694717521940989));
#12286=CARTESIAN_POINT('Ctrl Pts',(1.10000143498593,1.22871439246446,0.693103507978966));
#12287=CARTESIAN_POINT('Ctrl Pts',(1.10000166711622,1.23613807995602,0.690206957744321));
#12288=CARTESIAN_POINT('Ctrl Pts',(1.10000160692769,1.24318920265812,0.686469797174223));
#12289=CARTESIAN_POINT('Ctrl Pts',(1.10000129432656,1.24972159507123,0.681973692132557));
#12290=CARTESIAN_POINT('Ctrl Pts',(1.10000112259081,1.25331033895651,0.679503636989594));
#12291=CARTESIAN_POINT('Ctrl Pts',(1.10000088087184,1.25674225826706,0.676803638555143));
#12292=CARTESIAN_POINT('Ctrl Pts',(1.10000066684112,1.25998923415267,0.673881729486736));
#12293=CARTESIAN_POINT('Ctrl Pts',(1.100000457217,1.26316935916797,0.671019978599686));
#12294=CARTESIAN_POINT('Ctrl Pts',(1.1000002715704,1.26615273734033,0.667962699881477));
#12295=CARTESIAN_POINT('Ctrl Pts',(1.1000002731257,1.2689166530284,0.664721467295484));
#12296=CARTESIAN_POINT('Ctrl Pts',(1.10000027600127,1.2740268283512,0.658728785663437));
#12297=CARTESIAN_POINT('Ctrl Pts',(1.10000085014601,1.27838972527875,0.652108677049879));
#12298=CARTESIAN_POINT('Ctrl Pts',(1.1000010530947,1.28194599975408,0.64502688444408));
#12299=CARTESIAN_POINT('Ctrl Pts',(1.10000107362034,1.2823056710724,0.644310652415237));
#12300=CARTESIAN_POINT('Ctrl Pts',(1.10000109127028,1.28265705236355,0.643589678557342));
#12301=CARTESIAN_POINT('Ctrl Pts',(1.10000110571348,1.28300005475086,0.642864123553892));
#12302=CARTESIAN_POINT('Ctrl Pts',(1.10000124853573,1.28639184812822,0.635689442715943));
#12303=CARTESIAN_POINT('Ctrl Pts',(1.10000097361067,1.28892914698194,0.628151301589031));
#12304=CARTESIAN_POINT('Ctrl Pts',(1.10000056283738,1.29055881622654,0.620418355899457));
#12305=CARTESIAN_POINT('Ctrl Pts',(1.10000029930222,1.29160434466024,0.615457217544876));
#12306=CARTESIAN_POINT('Ctrl Pts',(1.0999999999818,1.29227543558766,0.610415225971447));
#12307=CARTESIAN_POINT('Ctrl Pts',(1.1000000000255,1.29254692753179,0.605334652628598));
#12308=CARTESIAN_POINT('',(1.10000000295569,-1.29254692766489,0.605334652628491));
#12309=CARTESIAN_POINT('Ctrl Pts',(1.1000000000255,-1.29254692753179,0.605334652628598));
#12310=CARTESIAN_POINT('Ctrl Pts',(1.09999999995744,-1.29212405100831,0.613248166229861));
#12311=CARTESIAN_POINT('Ctrl Pts',(1.10000066442022,-1.29073420569755,0.621070584654331));
#12312=CARTESIAN_POINT('Ctrl Pts',(1.10000095378343,-1.28846118610397,0.628641296001913));
#12313=CARTESIAN_POINT('Ctrl Pts',(1.10000111506646,-1.28719426797524,0.632861000698125));
#12314=CARTESIAN_POINT('Ctrl Pts',(1.10000118318417,-1.28565198202118,0.637002542581089));
#12315=CARTESIAN_POINT('Ctrl Pts',(1.10000113489265,-1.28384214455607,0.641036116698538));
#12316=CARTESIAN_POINT('Ctrl Pts',(1.10000104828677,-1.28059638744501,0.648269916488365));
#12317=CARTESIAN_POINT('Ctrl Pts',(1.10000053334783,-1.27652829029495,0.655078571385522));
#12318=CARTESIAN_POINT('Ctrl Pts',(1.10000033433257,-1.27170133822839,0.661298646557671));
#12319=CARTESIAN_POINT('Ctrl Pts',(1.10000029715544,-1.27079963749419,0.662460590217389));
#12320=CARTESIAN_POINT('Ctrl Pts',(1.10000027400485,-1.26987132743055,0.663601924550879));
#12321=CARTESIAN_POINT('Ctrl Pts',(1.10000027368829,-1.26891665304159,0.664721467295481));
#12322=CARTESIAN_POINT('Ctrl Pts',(1.10000027305905,-1.2670190620795,0.666946764442229));
#12323=CARTESIAN_POINT('Ctrl Pts',(1.10000036187052,-1.26501734165944,0.669086014589825));
#12324=CARTESIAN_POINT('Ctrl Pts',(1.10000048327469,-1.26291879257262,0.671135465892351));
#12325=CARTESIAN_POINT('Ctrl Pts',(1.10000081209565,-1.25723491092676,0.676686367091516));
#12326=CARTESIAN_POINT('Ctrl Pts',(1.10000132622062,-1.25090760500066,0.68151881845922));
#12327=CARTESIAN_POINT('Ctrl Pts',(1.10000150097561,-1.24410063152763,0.68557843671136));
#12328=CARTESIAN_POINT('Ctrl Pts',(1.10000161196703,-1.2397773464179,0.688156805381407));
#12329=CARTESIAN_POINT('Ctrl Pts',(1.1000016084534,-1.23525961544019,0.690422742497405));
#12330=CARTESIAN_POINT('Ctrl Pts',(1.10000148831111,-1.23058375131837,0.692353039195786));
#12331=CARTESIAN_POINT('Ctrl Pts',(1.10000130031927,-1.22326722442338,0.695373457954986));
#12332=CARTESIAN_POINT('Ctrl Pts',(1.1000008264887,-1.21564857658641,0.697539632783775));
#12333=CARTESIAN_POINT('Ctrl Pts',(1.10000044322439,-1.20787483729518,0.698781928831272));
#12334=CARTESIAN_POINT('Ctrl Pts',(1.1000001958084,-1.20285650563037,0.6995838921283));
#12335=CARTESIAN_POINT('Ctrl Pts',(1.1,-1.19777295102175,0.7));
#12336=CARTESIAN_POINT('Ctrl Pts',(1.1,-1.19266190204553,0.7));
#12337=CARTESIAN_POINT('',(1.1,-1.324891758307,0.));
#12338=CARTESIAN_POINT('Ctrl Pts',(1.1,-1.324891758307,0.));
#12339=CARTESIAN_POINT('Ctrl Pts',(1.1,-1.3195129727271,0.10067220872632));
#12340=CARTESIAN_POINT('Ctrl Pts',(1.1,-1.31413394019217,0.201345046154956));
#12341=CARTESIAN_POINT('Ctrl Pts',(1.1,-1.30335235623932,0.40312282767794));
#12342=CARTESIAN_POINT('Ctrl Pts',(1.10000000295569,-1.29794973349953,0.504229074424201));
#12343=CARTESIAN_POINT('Ctrl Pts',(1.10000000295569,-1.29254692766489,0.605334652628491));
#12344=CARTESIAN_POINT('',(1.1,-1.39290118819044,0.));
#12345=CARTESIAN_POINT('Origin',(0.199725906950915,-1.5,-0.0104671912485888));
#12346=CARTESIAN_POINT('',(0.200274469199584,1.20659878095028,0.));
#12347=CARTESIAN_POINT('',(0.200274469199585,-0.75,0.));
#12348=CARTESIAN_POINT('',(0.231993417893744,1.17491202960101,0.605233595624295));
#12349=CARTESIAN_POINT('Ctrl Pts',(0.200274469199584,1.20659878095028,-9.43255890062389E-18));
#12350=CARTESIAN_POINT('Ctrl Pts',(0.210847451958254,1.19603647956141,0.20174452921517));
#12351=CARTESIAN_POINT('Ctrl Pts',(0.221420434855641,1.18547422886796,0.403489061077219));
#12352=CARTESIAN_POINT('Ctrl Pts',(0.231993417893744,1.17491202960101,0.605233595624295));
#12353=CARTESIAN_POINT('',(0.231993417893744,-1.17491202960101,0.605233595624295));
#12354=CARTESIAN_POINT('',(0.231993417893744,-0.75,0.605233595624295));
#12355=CARTESIAN_POINT('',(0.200274469199584,-1.20659878095028,1.38777878078145E-17));
#12356=CARTESIAN_POINT('Ctrl Pts',(0.231993417893744,-1.17491202960101,
0.605233595624295));
#12357=CARTESIAN_POINT('Ctrl Pts',(0.221420434855641,-1.18547422886796,
0.40348906107722));
#12358=CARTESIAN_POINT('Ctrl Pts',(0.210847451958254,-1.19603647956141,
0.20174452921517));
#12359=CARTESIAN_POINT('Ctrl Pts',(0.200274469199584,-1.20659878095028,
2.0491421059976E-17));
#12360=CARTESIAN_POINT('',(0.200274469199585,-0.75,0.));
#12361=CARTESIAN_POINT('Origin',(6.87299528185878,-3.57834294608796E-18,
0.));
#12362=CARTESIAN_POINT('Ctrl Pts',(8.90000000000001,-1.62420669932031,-3.75133951679985E-17));
#12363=CARTESIAN_POINT('Ctrl Pts',(10.0682843079684,-1.69891080436391,-1.31961514553165E-7));
#12364=CARTESIAN_POINT('Ctrl Pts',(11.2345361392062,-1.79243531443695,-6.44452192334729E-8));
#12365=CARTESIAN_POINT('Ctrl Pts',(12.4000000002382,-1.91212902541327,2.95121624705651E-11));
#12366=CARTESIAN_POINT('Ctrl Pts',(12.4000000002382,1.91212902541327,2.95118849063386E-11));
#12367=CARTESIAN_POINT('Ctrl Pts',(11.2345361911441,1.79243531977099,-6.4445136166539E-8));
#12368=CARTESIAN_POINT('Ctrl Pts',(10.0682843567552,1.69891080748336,-1.31958638870612E-7));
#12369=CARTESIAN_POINT('Ctrl Pts',(8.9,1.62420669932031,6.39679281766448E-17));
#12370=CARTESIAN_POINT('',(8.7,1.61160179736194,0.));
#12371=CARTESIAN_POINT('',(8.7,1.68851851851852,0.));
#12372=CARTESIAN_POINT('Ctrl Pts',(8.70000000002062,1.61160179731554,-3.21507306454832E-13));
#12373=CARTESIAN_POINT('Ctrl Pts',(7.99734938728961,1.56795839277283,5.29471456843263E-9));
#12374=CARTESIAN_POINT('Ctrl Pts',(7.29393815910572,1.53097060499506,-6.44604909847991E-9));
#12375=CARTESIAN_POINT('Ctrl Pts',(6.58949465297818,1.49904250536939,-7.60372244394637E-9));
#12376=CARTESIAN_POINT('Ctrl Pts',(5.94302350041144,1.46974193664425,-8.66612477447903E-9));
#12377=CARTESIAN_POINT('Ctrl Pts',(5.29757001768168,1.44478244743454,1.79883147367388E-8));
#12378=CARTESIAN_POINT('Ctrl Pts',(4.65216233480351,1.42284617839366,3.84107779578714E-9));
#12379=CARTESIAN_POINT('Ctrl Pts',(4.60144142975536,1.4211222642714,2.72928337404163E-9));
#12380=CARTESIAN_POINT('Ctrl Pts',(4.55072080855761,1.41941704699729,1.44770501019496E-9));
#12381=CARTESIAN_POINT('Ctrl Pts',(4.50000000001737,1.41772989873549,-1.00876616052154E-12));
#12382=CARTESIAN_POINT('',(4.3,1.41116952203211,0.));
#12383=CARTESIAN_POINT('',(4.3,1.48481481481482,0.));
#12384=CARTESIAN_POINT('Ctrl Pts',(4.3,1.41116952203211,-1.0790522121662E-15));
#12385=CARTESIAN_POINT('Ctrl Pts',(3.23514221724601,1.37672428690534,3.20725535317031E-8));
#12386=CARTESIAN_POINT('Ctrl Pts',(2.16992716239601,1.34987955958158,4.63097810372671E-9));
#12387=CARTESIAN_POINT('Ctrl Pts',(1.10000000020726,1.32489175811528,-9.82792569252214E-12));
#12388=CARTESIAN_POINT('',(0.9,1.32024227787037,0.));
#12389=CARTESIAN_POINT('',(0.9,1.39290118819044,0.));
#12390=CARTESIAN_POINT('',(0.297857995688647,1.306435779838,0.));
#12391=CARTESIAN_POINT('Ctrl Pts',(0.9,1.32024227787037,-6.93889390390723E-18));
#12392=CARTESIAN_POINT('Ctrl Pts',(0.699470323836888,1.31560060380002,-4.72996299588896E-10));
#12393=CARTESIAN_POINT('Ctrl Pts',(0.498765843889866,1.3110112408976,-1.02277582142263E-13));
#12394=CARTESIAN_POINT('Ctrl Pts',(0.297857995688647,1.306435779838,-1.00157829096748E-16));
#12395=CARTESIAN_POINT('Ctrl Pts',(0.297857995688647,1.306435779838,-1.95156391047391E-17));
#12396=CARTESIAN_POINT('Ctrl Pts',(0.289922476296638,1.30625505685688,-1.46278605970555E-13));
#12397=CARTESIAN_POINT('Ctrl Pts',(0.282050301799808,1.30510306275878,-1.25203502999379E-6));
#12398=CARTESIAN_POINT('Ctrl Pts',(0.274405144964298,1.30305953674341,-1.39678564665046E-6));
#12399=CARTESIAN_POINT('Ctrl Pts',(0.269498922713003,1.30174811919849,-1.48967827287246E-6));
#12400=CARTESIAN_POINT('Ctrl Pts',(0.26468600784495,1.30006837070384,-1.17796618578504E-6));
#12401=CARTESIAN_POINT('Ctrl Pts',(0.260012701218123,1.29803054880949,-5.63923085528507E-7));
#12402=CARTESIAN_POINT('Ctrl Pts',(0.252740988282594,1.29485967708789,3.91534262267771E-7));
#12403=CARTESIAN_POINT('Ctrl Pts',(0.245891302634708,1.2908611961912,2.26944434681222E-6));
#12404=CARTESIAN_POINT('Ctrl Pts',(0.239629152465829,1.28609427281,1.73040332626933E-6));
#12405=CARTESIAN_POINT('Ctrl Pts',(0.238677421334952,1.28536978852616,1.6484790500646E-6));
#12406=CARTESIAN_POINT('Ctrl Pts',(0.23773930716971,1.28462746803483,1.50379952206709E-6));
#12407=CARTESIAN_POINT('Ctrl Pts',(0.236815449960777,1.28386742955246,1.27686598471174E-6));
#12408=CARTESIAN_POINT('Ctrl Pts',(0.233849259515119,1.28142720517261,5.48259784756267E-7));
#12409=CARTESIAN_POINT('Ctrl Pts',(0.231029859162728,1.27880446664625,-1.01231737317126E-6));
#12410=CARTESIAN_POINT('Ctrl Pts',(0.228365947504865,1.27601569667724,-2.73789903475208E-6));
#12411=CARTESIAN_POINT('Ctrl Pts',(0.222875659368053,1.2702680771449,-6.2943009513513E-6));
#12412=CARTESIAN_POINT('Ctrl Pts',(0.218108003769119,1.26388547870891,-1.02458913084139E-5));
#12413=CARTESIAN_POINT('Ctrl Pts',(0.214119068651703,1.25703104885628,-1.16727273233865E-5));
#12414=CARTESIAN_POINT('Ctrl Pts',(0.211608035823831,1.25271618840614,-1.25709199407453E-5));
#12415=CARTESIAN_POINT('Ctrl Pts',(0.209406266788438,1.24821342134138,-1.25531979180244E-5));
#12416=CARTESIAN_POINT('Ctrl Pts',(0.207536767894457,1.24355803714115,-1.16467700682383E-5));
#12417=CARTESIAN_POINT('Ctrl Pts',(0.204585779527196,1.23620955211972,-1.02159812889057E-5));
#12418=CARTESIAN_POINT('Ctrl Pts',(0.20249437279756,1.22856635796309,-6.44823334219156E-6));
#12419=CARTESIAN_POINT('Ctrl Pts',(0.201333199355162,1.22077498745768,-3.37414558979738E-6));
#12420=CARTESIAN_POINT('Ctrl Pts',(0.200635497716839,1.21609347152911,-1.5270519663277E-6));
#12421=CARTESIAN_POINT('Ctrl Pts',(0.200274469246579,1.21135795995708,-3.76748562593766E-12));
#12422=CARTESIAN_POINT('Ctrl Pts',(0.200274469199584,1.20659878095028,6.07153216591882E-18));
#12423=CARTESIAN_POINT('',(-2.81723893694256E-19,1.20714678905882,-2.77862675945125E-17));
#12424=CARTESIAN_POINT('',(0.,-1.5,0.));
#12425=CARTESIAN_POINT('',(0.292751161823634,1.50665779898694,0.));
#12426=CARTESIAN_POINT('Ctrl Pts',(0.292751161823634,1.50665779898694,-4.77048955893622E-17));
#12427=CARTESIAN_POINT('Ctrl Pts',(0.274916014309114,1.50625165707847,3.84528327419955E-12));
#12428=CARTESIAN_POINT('Ctrl Pts',(0.257184594685611,1.50420857033458,-2.03607170333744E-6));
#12429=CARTESIAN_POINT('Ctrl Pts',(0.239764500086274,1.50063675387888,-2.79213621391921E-6));
#12430=CARTESIAN_POINT('Ctrl Pts',(0.222116086584643,1.49701812291205,-3.55811018958082E-6));
#12431=CARTESIAN_POINT('Ctrl Pts',(0.204785660682177,1.49183000356027,-2.9511242418033E-6));
#12432=CARTESIAN_POINT('Ctrl Pts',(0.187998620502071,1.4851341555102,-6.80337370794577E-7));
#12433=CARTESIAN_POINT('Ctrl Pts',(0.185044527596802,1.48395585623842,-2.80736529130144E-7));
#12434=CARTESIAN_POINT('Ctrl Pts',(0.182107319868513,1.48273075079643,1.61255976403501E-7));
#12435=CARTESIAN_POINT('Ctrl Pts',(0.17918831289364,1.48145903083089,6.35063889779883E-7));
#12436=CARTESIAN_POINT('Ctrl Pts',(0.162608037952008,1.47423552404966,3.32634402063389E-6));
#12437=CARTESIAN_POINT('Ctrl Pts',(0.146760254055949,1.46557586252388,7.36741945499403E-6));
#12438=CARTESIAN_POINT('Ctrl Pts',(0.131860714325404,1.4555643673366,8.80872142158042E-6));
#12439=CARTESIAN_POINT('Ctrl Pts',(0.12416804976458,1.45039541073654,9.55286874158632E-6));
#12440=CARTESIAN_POINT('Ctrl Pts',(0.116728404005452,1.44486529627202,9.54902993357918E-6));
#12441=CARTESIAN_POINT('Ctrl Pts',(0.109574210210226,1.43898090192647,7.86258910610491E-6));
#12442=CARTESIAN_POINT('Ctrl Pts',(0.100675189791982,1.43166137062374,5.76484451217541E-6));
#12443=CARTESIAN_POINT('Ctrl Pts',(0.0922175942578585,1.42379373777092,
1.07962821494929E-6));
#12444=CARTESIAN_POINT('Ctrl Pts',(0.0842272493232774,1.41542759110015,
-4.17082519724513E-6));
#12445=CARTESIAN_POINT('Ctrl Pts',(0.0719003514327883,1.40252093480537,
-1.22708263387205E-5));
#12446=CARTESIAN_POINT('Ctrl Pts',(0.0607923942774574,1.38854365509349,
-2.1446290640466E-5));
#12447=CARTESIAN_POINT('Ctrl Pts',(0.0509667079859164,1.37370740939602,
-2.73088451608079E-5));
#12448=CARTESIAN_POINT('Ctrl Pts',(0.040988527714452,1.35864090617899,-3.32623861267576E-5));
#12449=CARTESIAN_POINT('Ctrl Pts',(0.0323319291028794,1.34268723517955,
-3.58272570146011E-5));
#12450=CARTESIAN_POINT('Ctrl Pts',(0.0251054147216294,1.32603775378173,
-3.42048160832586E-5));
#12451=CARTESIAN_POINT('Ctrl Pts',(0.0239557673766072,1.32338903116455,
-3.39467061825833E-5));
#12452=CARTESIAN_POINT('Ctrl Pts',(0.022842414085455,1.32072266145131,-3.35898145907185E-5));
#12453=CARTESIAN_POINT('Ctrl Pts',(0.0217659098422027,1.31803938112476,
-3.31388957009043E-5));
#12454=CARTESIAN_POINT('Ctrl Pts',(0.0146851456525434,1.30038996137917,
-3.01729526055095E-5));
#12455=CARTESIAN_POINT('Ctrl Pts',(0.00925910545076598,1.282173175788,-2.28911926108039E-5));
#12456=CARTESIAN_POINT('Ctrl Pts',(0.0055880418397064,1.26361786690427,
-1.53360241296986E-5));
#12457=CARTESIAN_POINT('Ctrl Pts',(0.00217213684284492,1.24635225152695,
-8.30598038733772E-6));
#12458=CARTESIAN_POINT('Ctrl Pts',(0.000275638047107462,1.2287919996398,
-1.11502351997496E-6));
#12459=CARTESIAN_POINT('Ctrl Pts',(2.78020181985954E-5,1.21111091902543,
-1.13803743790751E-7));
#12460=CARTESIAN_POINT('Ctrl Pts',(9.289355304618E-6,1.20979019141994,-3.90154078055202E-8));
#12461=CARTESIAN_POINT('Ctrl Pts',(3.5054796412911E-11,1.20846879032832,
-2.82152417201308E-12));
#12462=CARTESIAN_POINT('Ctrl Pts',(6.5594231435373E-18,1.20714678905882,
2.42861286636753E-17));
#12463=CARTESIAN_POINT('',(12.8678148030684,2.16300527278356,0.));
#12464=CARTESIAN_POINT('Ctrl Pts',(0.292751161823634,1.50665779898694,0.));
#12465=CARTESIAN_POINT('Ctrl Pts',(4.48443904223854,1.60211086545473,0.));
#12466=CARTESIAN_POINT('Ctrl Pts',(8.67612692265345,1.70561506876628,0.));
#12467=CARTESIAN_POINT('Ctrl Pts',(12.8678148030684,2.16300527278356,0.));
#12468=CARTESIAN_POINT('',(13.2,1.86519007666192,1.29914761427265E-16));
#12469=CARTESIAN_POINT('Ctrl Pts',(13.2,1.86519007666192,1.40512601554121E-16));
#12470=CARTESIAN_POINT('Ctrl Pts',(13.2000000013352,1.88296731840607,9.35191444695304E-11));
#12471=CARTESIAN_POINT('Ctrl Pts',(13.1983511006715,1.90064589040826,-4.81925060583158E-6));
#12472=CARTESIAN_POINT('Ctrl Pts',(13.1951709302004,1.91804121845656,-9.22684518112407E-6));
#12473=CARTESIAN_POINT('Ctrl Pts',(13.1919252271695,1.93579500539423,-1.37252653764835E-5));
#12474=CARTESIAN_POINT('Ctrl Pts',(13.1870840836913,1.95325521073227,-1.77396479500911E-5));
#12475=CARTESIAN_POINT('Ctrl Pts',(13.1807207319279,1.9702167899609,-1.88895599539727E-5));
#12476=CARTESIAN_POINT('Ctrl Pts',(13.179605107926,1.97319049715201,-1.90911627380646E-5));
#12477=CARTESIAN_POINT('Ctrl Pts',(13.1784425783122,1.97614882406338,-1.92137058190342E-5));
#12478=CARTESIAN_POINT('Ctrl Pts',(13.1772333926356,1.97909058504493,-1.92562174744009E-5));
#12479=CARTESIAN_POINT('Ctrl Pts',(13.1703491364924,1.99583891121373,-1.94982490583826E-5));
#12480=CARTESIAN_POINT('Ctrl Pts',(13.1620175712498,2.0119031422279,-1.67925698753361E-5));
#12481=CARTESIAN_POINT('Ctrl Pts',(13.1523342210936,2.02708796667103,-1.30402710852334E-5));
#12482=CARTESIAN_POINT('Ctrl Pts',(13.1443502942575,2.03960786168842,-9.94649893779315E-6));
#12483=CARTESIAN_POINT('Ctrl Pts',(13.1354462980072,2.05153020544825,-6.18593217696112E-6));
#12484=CARTESIAN_POINT('Ctrl Pts',(13.1256528604983,2.06273196126272,-4.73977425690188E-6));
#12485=CARTESIAN_POINT('Ctrl Pts',(13.1217453950533,2.06720132901318,-4.16277439392992E-6));
#12486=CARTESIAN_POINT('Ctrl Pts',(13.1176961215346,2.07155579183536,-3.97575052791371E-6));
#12487=CARTESIAN_POINT('Ctrl Pts',(13.1135113749213,2.07579033931164,-3.99023031318383E-6));
#12488=CARTESIAN_POINT('Ctrl Pts',(13.1009362730034,2.08851509208914,-4.03374185458576E-6));
#12489=CARTESIAN_POINT('Ctrl Pts',(13.0872516297578,2.10004749226926,-5.60236028337187E-6));
#12490=CARTESIAN_POINT('Ctrl Pts',(13.0726646436523,2.11028882659185,-6.03124820804926E-6));
#12491=CARTESIAN_POINT('Ctrl Pts',(13.0580194031224,2.12057106059247,-6.46184893473862E-6));
#12492=CARTESIAN_POINT('Ctrl Pts',(13.0424632957183,2.12955278528135,-5.76500392338198E-6));
#12493=CARTESIAN_POINT('Ctrl Pts',(13.0261754841647,2.13709349482706,-4.98347139369932E-6));
#12494=CARTESIAN_POINT('Ctrl Pts',(13.0233759049672,2.13838960594114,-4.84914013593099E-6));
#12495=CARTESIAN_POINT('Ctrl Pts',(13.0205546633935,2.13964302898522,-4.72077764982159E-6));
#12496=CARTESIAN_POINT('Ctrl Pts',(13.0177126224567,2.14085289970554,-4.61407510358037E-6));
#12497=CARTESIAN_POINT('Ctrl Pts',(13.0148367726024,2.14207716304734,-4.50610322390289E-6));
#12498=CARTESIAN_POINT('Ctrl Pts',(13.0119432782921,2.14325527660784,-4.42172619954107E-6));
#12499=CARTESIAN_POINT('Ctrl Pts',(13.0090331608036,2.14438664763146,-4.38057543634576E-6));
#12500=CARTESIAN_POINT('Ctrl Pts',(12.9922536897216,2.1509100294015,-4.14330390220891E-6));
#12501=CARTESIAN_POINT('Ctrl Pts',(12.9749229882599,2.15588345271621,-5.05640020348117E-6));
#12502=CARTESIAN_POINT('Ctrl Pts',(12.9572550825995,2.15928949382789,-4.85686529648217E-6));
#12503=CARTESIAN_POINT('Ctrl Pts',(12.9529252316797,2.16012420794307,-4.80796553341985E-6));
#12504=CARTESIAN_POINT('Ctrl Pts',(12.9485750628159,2.16086455090717,-4.70814629363608E-6));
#12505=CARTESIAN_POINT('Ctrl Pts',(12.944207640703,2.16150979950679,-4.55317442353944E-6));
#12506=CARTESIAN_POINT('Ctrl Pts',(12.9263774359968,2.16414405704371,-3.92049452767182E-6));
#12507=CARTESIAN_POINT('Ctrl Pts',(12.9083632163621,2.16518216214944,-2.15504024707585E-6));
#12508=CARTESIAN_POINT('Ctrl Pts',(12.8903762705535,2.16459816844574,-9.12104093693782E-7));
#12509=CARTESIAN_POINT('Ctrl Pts',(12.8828459063217,2.16435367528137,-3.91739933400607E-7));
#12510=CARTESIAN_POINT('Ctrl Pts',(12.8753202361859,2.1638242536466,5.87463683432524E-12));
#12511=CARTESIAN_POINT('Ctrl Pts',(12.8678148030684,2.16300527278357,2.8796409701215E-16));
#12512=CARTESIAN_POINT('',(13.2,-1.86519007666192,1.11326398357188E-16));
#12513=CARTESIAN_POINT('',(13.2,2.2,0.));
#12514=CARTESIAN_POINT('',(12.8678148030684,-2.16300527278356,1.38777878078145E-17));
#12515=CARTESIAN_POINT('Ctrl Pts',(12.8678148030684,-2.16300527278357,2.56739074444567E-16));
#12516=CARTESIAN_POINT('Ctrl Pts',(12.8854929372559,-2.16493428409685,8.24591542686399E-11));
#12517=CARTESIAN_POINT('Ctrl Pts',(12.9032520674897,-2.16521372082443,-4.52295339524789E-6));
#12518=CARTESIAN_POINT('Ctrl Pts',(12.9208958607904,-2.1639404182545,-8.68231213275745E-6));
#12519=CARTESIAN_POINT('Ctrl Pts',(12.9389012534027,-2.16264102008682,-1.29269145154966E-5));
#12520=CARTESIAN_POINT('Ctrl Pts',(12.9567880250381,-2.15972433317902,-1.67278855193166E-5));
#12521=CARTESIAN_POINT('Ctrl Pts',(12.9743443410528,-2.15524079327399,-1.78237954457702E-5));
#12522=CARTESIAN_POINT('Ctrl Pts',(12.9774431846623,-2.15444940919484,-1.80172331504298E-5));
#12523=CARTESIAN_POINT('Ctrl Pts',(12.9805316913262,-2.15360908525727,-1.81351031595367E-5));
#12524=CARTESIAN_POINT('Ctrl Pts',(12.9836086301392,-2.15271994254544,-1.81766625580856E-5));
#12525=CARTESIAN_POINT('Ctrl Pts',(13.0010041030966,-2.14769317440371,-1.84116186093898E-5));
#12526=CARTESIAN_POINT('Ctrl Pts',(13.017876958431,-2.14115457229109,-1.5854618169158E-5));
#12527=CARTESIAN_POINT('Ctrl Pts',(13.0340226638693,-2.13317744288338,-1.23136839993165E-5));
#12528=CARTESIAN_POINT('Ctrl Pts',(13.0473215411186,-2.12660684953271,-9.39709115965876E-6));
#12529=CARTESIAN_POINT('Ctrl Pts',(13.060127470267,-2.11905920305061,-5.85016632862467E-6));
#12530=CARTESIAN_POINT('Ctrl Pts',(13.0723151314263,-2.11055132433008,-4.53327195050794E-6));
#12531=CARTESIAN_POINT('Ctrl Pts',(13.0772147086919,-2.10713106111368,-4.00386555564548E-6));
#12532=CARTESIAN_POINT('Ctrl Pts',(13.0820141951123,-2.10355537352593,-3.85636210984559E-6));
#12533=CARTESIAN_POINT('Ctrl Pts',(13.0867078006727,-2.0998301147952,-3.90248451975241E-6));
#12534=CARTESIAN_POINT('Ctrl Pts',(13.1007249787291,-2.08870484782034,-4.04022639510273E-6));
#12535=CARTESIAN_POINT('Ctrl Pts',(13.1136765748478,-2.07634683247102,-5.5945154994439E-6));
#12536=CARTESIAN_POINT('Ctrl Pts',(13.1254414850725,-2.06295113861397,-5.97495381195624E-6));
#12537=CARTESIAN_POINT('Ctrl Pts',(13.1372476314214,-2.04950849272046,-6.35672556443159E-6));
#12538=CARTESIAN_POINT('Ctrl Pts',(13.1478597809499,-2.03501968083851,-5.56609061204695E-6));
#12539=CARTESIAN_POINT('Ctrl Pts',(13.1571184147632,-2.01964723728874,-4.75455255839871E-6));
#12540=CARTESIAN_POINT('Ctrl Pts',(13.158708901902,-2.01700649414547,-4.61514313115074E-6));
#12541=CARTESIAN_POINT('Ctrl Pts',(13.1602593369672,-2.01433961799121,-4.48389992381974E-6));
#12542=CARTESIAN_POINT('Ctrl Pts',(13.1617687665475,-2.01164737048868,-4.37752847101542E-6));
#12543=CARTESIAN_POINT('Ctrl Pts',(13.1632768494098,-2.00895752501823,-4.27125192317111E-6));
#12544=CARTESIAN_POINT('Ctrl Pts',(13.164742106841,-2.00624572954308,-4.19089851494128E-6));
#12545=CARTESIAN_POINT('Ctrl Pts',(13.1661638648313,-2.00351289682408,-4.15637526360595E-6));
#12546=CARTESIAN_POINT('Ctrl Pts',(13.1744716670281,-1.98754405133797,-3.95464448717833E-6));
#12547=CARTESIAN_POINT('Ctrl Pts',(13.181298057795,-1.97085874357403,-5.01850453361653E-6));
#12548=CARTESIAN_POINT('Ctrl Pts',(13.1866022393826,-1.95366776591112,-4.89891140766866E-6));
#12549=CARTESIAN_POINT('Ctrl Pts',(13.1879075264936,-1.94943729958961,-4.86948116225E-6));
#12550=CARTESIAN_POINT('Ctrl Pts',(13.1891204013114,-1.94517611908519,-4.78523710928743E-6));
#12551=CARTESIAN_POINT('Ctrl Pts',(13.1902397948733,-1.94088722910442,-4.64104147683466E-6));
#12552=CARTESIAN_POINT('Ctrl Pts',(13.1947901580114,-1.92345278286841,-4.05488258426869E-6));
#12553=CARTESIAN_POINT('Ctrl Pts',(13.1977733658442,-1.90566244769967,-2.24449026644408E-6));
#12554=CARTESIAN_POINT('Ctrl Pts',(13.1991406030032,-1.88772335428786,-9.50757284845071E-7));
#12555=CARTESIAN_POINT('Ctrl Pts',(13.1997114533543,-1.8802334044254,-4.10596478211383E-7));
#12556=CARTESIAN_POINT('Ctrl Pts',(13.2000000000958,-1.87271737110067,6.9401096738129E-12));
#12557=CARTESIAN_POINT('Ctrl Pts',(13.2,-1.86519007666192,1.81278603239576E-16));
#12558=CARTESIAN_POINT('',(0.292751161823634,-1.50665779898694,-1.38777878078145E-17));
#12559=CARTESIAN_POINT('Ctrl Pts',(12.8678148030684,-2.16300527278356,0.));
#12560=CARTESIAN_POINT('Ctrl Pts',(8.67612692265345,-1.70561506876628,0.));
#12561=CARTESIAN_POINT('Ctrl Pts',(4.48443904223854,-1.60211086545473,0.));
#12562=CARTESIAN_POINT('Ctrl Pts',(0.292751161823634,-1.50665779898694,
0.));
#12563=CARTESIAN_POINT('',(4.02814324098787E-18,-1.20714678905882,5.54818711994559E-17));
#12564=CARTESIAN_POINT('Ctrl Pts',(-2.22044604925031E-16,-1.20714678905882,
-3.98986399474666E-17));
#12565=CARTESIAN_POINT('Ctrl Pts',(2.12382277713531E-10,-1.2249878157372,
-1.35440422383976E-12));
#12566=CARTESIAN_POINT('Ctrl Pts',(0.00163882612763064,-1.24276245549475,
-1.96699749426327E-6));
#12567=CARTESIAN_POINT('Ctrl Pts',(0.00481304415265273,-1.26026068126938,
-2.66007142975038E-6));
#12568=CARTESIAN_POINT('Ctrl Pts',(0.00802873944670128,-1.27798755504872,
-3.36220171040687E-6));
#12569=CARTESIAN_POINT('Ctrl Pts',(0.0128206026099745,-1.29543230475431,
-2.69550948014298E-6));
#12570=CARTESIAN_POINT('Ctrl Pts',(0.0191320595672371,-1.31236817798419,
-4.00401478067381E-7));
#12571=CARTESIAN_POINT('Ctrl Pts',(0.0202443702650641,-1.31535290133701,
4.0809101773195E-9));
#12572=CARTESIAN_POINT('Ctrl Pts',(0.0214039964883031,-1.3183217636574,
4.5005107558061E-7));
#12573=CARTESIAN_POINT('Ctrl Pts',(0.0226107760969305,-1.32127343934773,
9.26779280916758E-7));
#12574=CARTESIAN_POINT('Ctrl Pts',(0.0294548697216842,-1.33801348419941,
3.63048130534217E-6));
#12575=CARTESIAN_POINT('Ctrl Pts',(0.0377511831708778,-1.35405403406083,
7.64722139837078E-6));
#12576=CARTESIAN_POINT('Ctrl Pts',(0.0474204318104353,-1.36917746582299,
9.03443059383348E-6));
#12577=CARTESIAN_POINT('Ctrl Pts',(0.0524109755304394,-1.37698305136733,
9.75040433665629E-6));
#12578=CARTESIAN_POINT('Ctrl Pts',(0.0577680562174045,-1.38454410063597,
9.71159147480002E-6));
#12579=CARTESIAN_POINT('Ctrl Pts',(0.0634855547170043,-1.39182806229354,
7.98761394269614E-6));
#12580=CARTESIAN_POINT('Ctrl Pts',(0.0706048733905122,-1.40089791062835,
5.84095042579577E-6));
#12581=CARTESIAN_POINT('Ctrl Pts',(0.0782829434694699,-1.40953838460506,
1.09773645972912E-6));
#12582=CARTESIAN_POINT('Ctrl Pts',(0.0864706998703675,-1.41772246232928,
-4.21049985396393E-6));
#12583=CARTESIAN_POINT('Ctrl Pts',(0.0990944981487371,-1.43034058886193,
-1.2394683793612E-5));
#12584=CARTESIAN_POINT('Ctrl Pts',(0.112816484288725,-1.44176429483685,
-2.16481703631134E-5));
#12585=CARTESIAN_POINT('Ctrl Pts',(0.127426518150943,-1.45192534842919,
-2.7562374581111E-5));
#12586=CARTESIAN_POINT('Ctrl Pts',(0.142261949549145,-1.46224316253723,
-3.35678206860622E-5));
#12587=CARTESIAN_POINT('Ctrl Pts',(0.158014355623482,-1.47125989363127,
-3.6155642403295E-5));
#12588=CARTESIAN_POINT('Ctrl Pts',(0.17449494651519,-1.47886261331763,-3.45187637154371E-5));
#12589=CARTESIAN_POINT('Ctrl Pts',(0.177115379630184,-1.48007145458801,
-3.42584981007467E-5));
#12590=CARTESIAN_POINT('Ctrl Pts',(0.179754261386328,-1.48124444832217,
-3.38986806574493E-5));
#12591=CARTESIAN_POINT('Ctrl Pts',(0.18241086941249,-1.48238102342202,-3.34441145409493E-5));
#12592=CARTESIAN_POINT('Ctrl Pts',(0.199890279181845,-1.48985922935543,
-3.04532527580594E-5));
#12593=CARTESIAN_POINT('Ctrl Pts',(0.217974246898519,-1.49569663469242,
-2.31073027206853E-5));
#12594=CARTESIAN_POINT('Ctrl Pts',(0.236436446036386,-1.49978781870256,
-1.54828395726751E-5));
#12595=CARTESIAN_POINT('Ctrl Pts',(0.253618559172887,-1.50359533838099,
-8.38702246898572E-6));
#12596=CARTESIAN_POINT('Ctrl Pts',(0.271129804961754,-1.50589051664322,
-1.1237837803371E-6));
#12597=CARTESIAN_POINT('Ctrl Pts',(0.288799387895208,-1.50654014509364,
-1.14426782679271E-7));
#12598=CARTESIAN_POINT('Ctrl Pts',(0.290115790923368,-1.5065885431154,-3.92285953074499E-8));
#12599=CARTESIAN_POINT('Ctrl Pts',(0.291433072638222,-1.50662778343727,
-2.32210426557352E-12));
#12600=CARTESIAN_POINT('Ctrl Pts',(0.292751161823634,-1.50665779898694,
2.86229373536173E-17));
#12601=CARTESIAN_POINT('',(0.,-1.5,0.));
#12602=CARTESIAN_POINT('',(0.297857995688647,-1.306435779838,0.));
#12603=CARTESIAN_POINT('Ctrl Pts',(0.200274469199585,-1.20659878095028,
-5.63785129692462E-18));
#12604=CARTESIAN_POINT('Ctrl Pts',(0.200274469233139,-1.21453676310593,
-8.71436967499621E-13));
#12605=CARTESIAN_POINT('Ctrl Pts',(0.201246859971722,-1.22243356087926,
-1.21395871814677E-6));
#12606=CARTESIAN_POINT('Ctrl Pts',(0.203115675186186,-1.23012372049816,
-1.3343733317444E-6));
#12607=CARTESIAN_POINT('Ctrl Pts',(0.204315340901654,-1.23506033529553,
-1.41167219064517E-6));
#12608=CARTESIAN_POINT('Ctrl Pts',(0.20588557457721,-1.23991201018842,-1.08820351238587E-6));
#12609=CARTESIAN_POINT('Ctrl Pts',(0.207817175189242,-1.24463217458037,
-4.7123943162984E-7));
#12610=CARTESIAN_POINT('Ctrl Pts',(0.210821635148072,-1.25197403646754,
4.8840194822981E-7));
#12611=CARTESIAN_POINT('Ctrl Pts',(0.214662962735955,-1.25891288736431,
2.34840446672759E-6));
#12612=CARTESIAN_POINT('Ctrl Pts',(0.219285851586231,-1.26528190572196,
1.77850405974346E-6));
#12613=CARTESIAN_POINT('Ctrl Pts',(0.219987799701267,-1.26624898941694,
1.69196931287913E-6));
#12614=CARTESIAN_POINT('Ctrl Pts',(0.220707854727247,-1.26720289123473,
1.54254180957111E-6));
#12615=CARTESIAN_POINT('Ctrl Pts',(0.221445913570039,-1.26814297034805,
1.31084431541716E-6));
#12616=CARTESIAN_POINT('Ctrl Pts',(0.223819423285066,-1.27116615329633,
5.65732650279818E-7));
#12617=CARTESIAN_POINT('Ctrl Pts',(0.226378993511503,-1.27404655624932,
-1.0141799309673E-6));
#12618=CARTESIAN_POINT('Ctrl Pts',(0.229108317341547,-1.27677508245113,
-2.75886047820546E-6));
#12619=CARTESIAN_POINT('Ctrl Pts',(0.234729699316268,-1.28239482161129,
-6.35224711555937E-6));
#12620=CARTESIAN_POINT('Ctrl Pts',(0.241002345945823,-1.28730653457646,
-1.03364935932408E-5));
#12621=CARTESIAN_POINT('Ctrl Pts',(0.247764463424355,-1.29145035967733,
-1.17765252099068E-5));
#12622=CARTESIAN_POINT('Ctrl Pts',(0.25202072563572,-1.29405859685204,-1.26829206064147E-5));
#12623=CARTESIAN_POINT('Ctrl Pts',(0.25647185453211,-1.29636195369988,-1.26655904667795E-5));
#12624=CARTESIAN_POINT('Ctrl Pts',(0.261083107941716,-1.29833661269995,
-1.17517412599227E-5));
#12625=CARTESIAN_POINT('Ctrl Pts',(0.268362152520619,-1.30145368947124,
-1.0309194402435E-5));
#12626=CARTESIAN_POINT('Ctrl Pts',(0.275955349537693,-1.30371808689536,
-6.50743389458559E-6));
#12627=CARTESIAN_POINT('Ctrl Pts',(0.283717840216357,-1.30505580179168,
-3.40467605837577E-6));
#12628=CARTESIAN_POINT('Ctrl Pts',(0.288379557365255,-1.3058591584372,-1.54133347766382E-6));
#12629=CARTESIAN_POINT('Ctrl Pts',(0.293102847896135,-1.30632748638856,
-3.09915230996644E-12));
#12630=CARTESIAN_POINT('Ctrl Pts',(0.297857995688647,-1.306435779838,2.90566182226115E-17));
#12631=CARTESIAN_POINT('',(0.9,-1.32024227787037,0.));
#12632=CARTESIAN_POINT('Ctrl Pts',(0.297857995688651,-1.306435779838,-5.81335652359571E-17));
#12633=CARTESIAN_POINT('Ctrl Pts',(0.498765834064439,-1.31101124067384,
-1.02216845336465E-13));
#12634=CARTESIAN_POINT('Ctrl Pts',(0.699470314209512,-1.31560060357718,
-4.73070532165219E-10));
#12635=CARTESIAN_POINT('Ctrl Pts',(0.9,-1.32024227787037,4.62320796019307E-17));
#12636=CARTESIAN_POINT('',(0.9,1.39290118819044,0.));
#12637=CARTESIAN_POINT('',(4.3,-1.41116952203211,0.));
#12638=CARTESIAN_POINT('Ctrl Pts',(1.10000000020724,-1.32489175811528,-9.82782277325449E-12));
#12639=CARTESIAN_POINT('Ctrl Pts',(2.16992692797068,-1.34987955410658,4.63225598025733E-9));
#12640=CARTESIAN_POINT('Ctrl Pts',(3.23514201430925,-1.37672428034078,3.20747301048384E-8));
#12641=CARTESIAN_POINT('Ctrl Pts',(4.3,-1.41116952203211,-8.74629427996717E-16));
#12642=CARTESIAN_POINT('',(4.3,1.48481481481482,0.));
#12643=CARTESIAN_POINT('',(8.7,-1.61160179736194,0.));
#12644=CARTESIAN_POINT('Ctrl Pts',(4.50000000001737,-1.41772989873549,-1.00870158580013E-12));
#12645=CARTESIAN_POINT('Ctrl Pts',(5.14541122039116,-1.43919849219739,1.84287460122322E-8));
#12646=CARTESIAN_POINT('Ctrl Pts',(5.79079200637672,-1.46358894290692,-2.29215846350395E-9));
#12647=CARTESIAN_POINT('Ctrl Pts',(6.43711407552466,-1.49221504703413,-7.12038357450289E-9));
#12648=CARTESIAN_POINT('Ctrl Pts',(6.48784335049204,-1.49446188584227,-7.49934689782436E-9));
#12649=CARTESIAN_POINT('Ctrl Pts',(6.5385784252675,-1.49673484630497,-7.6873350528488E-9));
#12650=CARTESIAN_POINT('Ctrl Pts',(6.58931977021612,-1.49903457911226,-7.60400982311631E-9));
#12651=CARTESIAN_POINT('Ctrl Pts',(7.29382172663923,-1.5309644828944,-6.44710735180711E-9));
#12652=CARTESIAN_POINT('Ctrl Pts',(7.99729122590638,-1.56795478022256,5.29179522587699E-9));
#12653=CARTESIAN_POINT('Ctrl Pts',(8.70000000002062,-1.61160179731554,-3.21479112539667E-13));
#12654=CARTESIAN_POINT('',(8.7,1.68851851851852,0.));
#12655=CARTESIAN_POINT('',(12.6,-1.93292824674167,0.));
#12656=CARTESIAN_POINT('',(12.8889963716306,-1.96391015057091,0.));
#12657=CARTESIAN_POINT('Ctrl Pts',(12.6000000004653,-1.93292824679067,-1.00288700954909E-16));
#12658=CARTESIAN_POINT('Ctrl Pts',(12.6963367945484,-1.94307238002033,2.28133307867826E-10));
#12659=CARTESIAN_POINT('Ctrl Pts',(12.7926686848896,-1.9533982851754,-5.07154825701885E-13));
#12660=CARTESIAN_POINT('Ctrl Pts',(12.8889963716306,-1.96391015057091,2.24786696790336E-16));
#12661=CARTESIAN_POINT('',(12.9997255308004,-1.86463850151065,-1.38777878078145E-17));
#12662=CARTESIAN_POINT('Ctrl Pts',(12.8889963716306,-1.96391015057091,5.29090660172926E-17));
#12663=CARTESIAN_POINT('Ctrl Pts',(12.8968843421745,-1.96477093437063,1.28387508960266E-11));
#12664=CARTESIAN_POINT('Ctrl Pts',(12.9048206871516,-1.96464841285931,-2.5989605143924E-6));
#12665=CARTESIAN_POINT('Ctrl Pts',(12.9126487282508,-1.9636130141884,-4.24292438262167E-6));
#12666=CARTESIAN_POINT('Ctrl Pts',(12.9176900487482,-1.96294620923983,-5.30165014054907E-6));
#12667=CARTESIAN_POINT('Ctrl Pts',(12.9226867577298,-1.96189962975099,-6.00943773338864E-6));
#12668=CARTESIAN_POINT('Ctrl Pts',(12.9275953864907,-1.96048085896027,-6.09358828708331E-6));
#12669=CARTESIAN_POINT('Ctrl Pts',(12.9352257743335,-1.95827540160737,-6.22439902734509E-6));
#12670=CARTESIAN_POINT('Ctrl Pts',(12.9425549137553,-1.95519874430406,-4.64402662178521E-6));
#12671=CARTESIAN_POINT('Ctrl Pts',(12.949425376669,-1.9513005478593,-3.15156624759025E-6));
#12672=CARTESIAN_POINT('Ctrl Pts',(12.9520760960011,-1.94979656991686,-2.57575445499556E-6));
#12673=CARTESIAN_POINT('Ctrl Pts',(12.9546583803074,-1.94816978416017,-2.04880625960079E-6));
#12674=CARTESIAN_POINT('Ctrl Pts',(12.9571622133441,-1.9464211898676,-1.82278374303809E-6));
#12675=CARTESIAN_POINT('Ctrl Pts',(12.9587955877505,-1.9452804951316,-1.67533805140214E-6));
#12676=CARTESIAN_POINT('Ctrl Pts',(12.9603955609302,-1.94408794089591,-1.65796127395168E-6));
#12677=CARTESIAN_POINT('Ctrl Pts',(12.9619602112942,-1.94284549575182,-1.70649031798611E-6));
#12678=CARTESIAN_POINT('Ctrl Pts',(12.9681665721336,-1.93791719798967,-1.89898620422551E-6));
#12679=CARTESIAN_POINT('Ctrl Pts',(12.9737470546445,-1.93226498850035,-2.8025064238469E-6));
#12680=CARTESIAN_POINT('Ctrl Pts',(12.9786034821464,-1.926037248212,-2.79230211737029E-6));
#12681=CARTESIAN_POINT('Ctrl Pts',(12.9817011960737,-1.92206483066456,-2.78579321297956E-6));
#12682=CARTESIAN_POINT('Ctrl Pts',(12.9845038017717,-1.91785723501915,-2.48811564693169E-6));
#12683=CARTESIAN_POINT('Ctrl Pts',(12.9869771252785,-1.91344616543364,-2.2918341012218E-6));
#12684=CARTESIAN_POINT('Ctrl Pts',(12.9874796596041,-1.91254991636901,-2.25195326317628E-6));
#12685=CARTESIAN_POINT('Ctrl Pts',(12.9879679417815,-1.9116463809131,-2.21866365029432E-6));
#12686=CARTESIAN_POINT('Ctrl Pts',(12.98844174868,-1.91073586520696,-2.19841011183313E-6));
#12687=CARTESIAN_POINT('Ctrl Pts',(12.9918929665356,-1.9041036526468,-2.05088297829219E-6));
#12688=CARTESIAN_POINT('Ctrl Pts',(12.9945793344589,-1.89710244289626,-2.35789128083535E-6));
#12689=CARTESIAN_POINT('Ctrl Pts',(12.9964698429198,-1.88986530397042,-1.93853625224654E-6));
#12690=CARTESIAN_POINT('Ctrl Pts',(12.9984668213505,-1.88222058265133,-1.49556391743615E-6));
#12691=CARTESIAN_POINT('Ctrl Pts',(12.9995610814633,-1.87437060764114,-2.4459616079733E-7));
#12692=CARTESIAN_POINT('Ctrl Pts',(12.9997084424383,-1.86646992060833,-2.60951667192209E-8));
#12693=CARTESIAN_POINT('Ctrl Pts',(12.9997198235207,-1.86585972940924,-9.21975031242219E-9));
#12694=CARTESIAN_POINT('Ctrl Pts',(12.9997255308031,-1.86524923282631,2.14479566203628E-13));
#12695=CARTESIAN_POINT('Ctrl Pts',(12.9997255308004,-1.86463850151065,-9.54097911787244E-18));
#12696=CARTESIAN_POINT('',(12.9997255308004,1.86463850151064,1.38777878078145E-17));
#12697=CARTESIAN_POINT('',(12.9997255308004,1.1,0.));
#12698=CARTESIAN_POINT('',(12.8889963716306,1.96391015057091,0.));
#12699=CARTESIAN_POINT('Ctrl Pts',(12.9997255308004,1.86463850151065,-9.97465998686664E-18));
#12700=CARTESIAN_POINT('Ctrl Pts',(12.9997255309996,1.87257112921612,1.42345874390777E-11));
#12701=CARTESIAN_POINT('Ctrl Pts',(12.9987425107347,1.88044501776258,-2.76622459581243E-6));
#12702=CARTESIAN_POINT('Ctrl Pts',(12.9968635501128,1.8881121101061,-4.50602169498049E-6));
#12703=CARTESIAN_POINT('Ctrl Pts',(12.9956551765012,1.89304287446485,-5.62489820561454E-6));
#12704=CARTESIAN_POINT('Ctrl Pts',(12.994075066483,1.89788828888188,-6.37205869803057E-6));
#12705=CARTESIAN_POINT('Ctrl Pts',(12.9921354490207,1.90260616696402,-6.45954116508302E-6));
#12706=CARTESIAN_POINT('Ctrl Pts',(12.9891151690915,1.90995262200289,-6.59576469602218E-6));
#12707=CARTESIAN_POINT('Ctrl Pts',(12.9852608829945,1.91690476599405,-4.92589918404109E-6));
#12708=CARTESIAN_POINT('Ctrl Pts',(12.9806393828366,1.92331154882078,-3.3382766296878E-6));
#12709=CARTESIAN_POINT('Ctrl Pts',(12.9788533632605,1.92578750666072,-2.72472586378502E-6));
#12710=CARTESIAN_POINT('Ctrl Pts',(12.9769522584487,1.92818179997524,-2.1610482659023E-6));
#12711=CARTESIAN_POINT('Ctrl Pts',(12.9749381758772,1.93048453804291,-1.90960564360578E-6));
#12712=CARTESIAN_POINT('Ctrl Pts',(12.9736352090466,1.93197424425657,-1.74694031832382E-6));
#12713=CARTESIAN_POINT('Ctrl Pts',(12.9722849384098,1.93342561524533,-1.71698229815602E-6));
#12714=CARTESIAN_POINT('Ctrl Pts',(12.9708894910408,1.9348369915754,-1.75552529092739E-6));
#12715=CARTESIAN_POINT('Ctrl Pts',(12.9653179015399,1.94047218048862,-1.90941553332435E-6));
#12716=CARTESIAN_POINT('Ctrl Pts',(12.9590944588136,1.94540670303376,-2.83773366290493E-6));
#12717=CARTESIAN_POINT('Ctrl Pts',(12.9523775255978,1.94955941520082,-2.8574013135715E-6));
#12718=CARTESIAN_POINT('Ctrl Pts',(12.9480923984168,1.95220867479748,-2.86994846593266E-6));
#12719=CARTESIAN_POINT('Ctrl Pts',(12.9436054681019,1.95453912223498,-2.59559485065602E-6));
#12720=CARTESIAN_POINT('Ctrl Pts',(12.9389519978263,1.95652032281755,-2.39773084743613E-6));
#12721=CARTESIAN_POINT('Ctrl Pts',(12.9379934875219,1.95692840561619,-2.35697530915642E-6));
#12722=CARTESIAN_POINT('Ctrl Pts',(12.9370291206935,1.95732112306527,-2.32193094846859E-6));
#12723=CARTESIAN_POINT('Ctrl Pts',(12.9360592398442,1.95769827921557,-2.29894501965994E-6));
#12724=CARTESIAN_POINT('Ctrl Pts',(12.929096105975,1.96040602292032,-2.13392052256244E-6));
#12725=CARTESIAN_POINT('Ctrl Pts',(12.9218497638689,1.96231496375013,-2.36509085467933E-6));
#12726=CARTESIAN_POINT('Ctrl Pts',(12.9144555496645,1.96340894166242,-1.92146179377921E-6));
#12727=CARTESIAN_POINT('Ctrl Pts',(12.9066371708262,1.96456567495722,-1.45238421961943E-6));
#12728=CARTESIAN_POINT('Ctrl Pts',(12.8987125532455,1.96480297730229,-2.37321368026999E-7));
#12729=CARTESIAN_POINT('Ctrl Pts',(12.8908401755085,1.96409377829808,-2.55627471131237E-8));
#12730=CARTESIAN_POINT('Ctrl Pts',(12.89022523009,1.96403837970149,-9.02136684357828E-9));
#12731=CARTESIAN_POINT('Ctrl Pts',(12.8896106033158,1.96397717928728,1.9621770460073E-13));
#12732=CARTESIAN_POINT('Ctrl Pts',(12.8889963716306,1.96391015057091,-3.29597460435593E-17));
#12733=CARTESIAN_POINT('',(12.6,1.93292824674167,0.));
#12734=CARTESIAN_POINT('Ctrl Pts',(12.8889963716306,1.96391015057091,8.95144418658345E-17));
#12735=CARTESIAN_POINT('Ctrl Pts',(12.7926686852738,1.95339828521733,-5.07275478770449E-13));
#12736=CARTESIAN_POINT('Ctrl Pts',(12.6963367949308,1.94307238006059,2.28132759158623E-10));
#12737=CARTESIAN_POINT('Ctrl Pts',(12.6000000004652,1.93292824679066,-1.5019386425618E-16));
#12738=CARTESIAN_POINT('',(12.6,-1.99376954809806,0.));
#12739=CARTESIAN_POINT('Origin',(11.2,0.,0.));
#12740=CARTESIAN_POINT('',(10.8,-4.89858719658942E-17,0.7));
#12741=CARTESIAN_POINT('Origin',(11.2,0.,0.7));
#12742=CARTESIAN_POINT('',(10.8,-4.89858719658942E-17,0.));
#12743=CARTESIAN_POINT('Origin',(2.,0.,0.));
#12744=CARTESIAN_POINT('',(1.6,-4.89858719658941E-17,0.));
#12745=CARTESIAN_POINT('Origin',(12.6,-1.99376954809806,0.));
#12746=CARTESIAN_POINT('',(12.6,-1.90428042248893,0.60470250816874));
#12747=CARTESIAN_POINT('Ctrl Pts',(12.6,-1.93292824674167,0.));
#12748=CARTESIAN_POINT('Ctrl Pts',(12.6,-1.92814118331811,0.100975624959503));
#12749=CARTESIAN_POINT('Ctrl Pts',(12.6,-1.9233557423333,0.20195205683881));
#12750=CARTESIAN_POINT('Ctrl Pts',(12.6,-1.91380649287245,0.40351907263528));
#12751=CARTESIAN_POINT('Ctrl Pts',(12.6,-1.90904260275794,0.504111110768618));
#12752=CARTESIAN_POINT('Ctrl Pts',(12.6,-1.90428042248893,0.60470250816874));
#12753=CARTESIAN_POINT('',(12.6,1.90428042248893,0.60470250816874));
#12754=CARTESIAN_POINT('Ctrl Pts',(12.6,1.90428042248893,0.60470250816874));
#12755=CARTESIAN_POINT('Ctrl Pts',(12.6,1.90904310126474,0.504100580823831));
#12756=CARTESIAN_POINT('Ctrl Pts',(12.6,1.91380749024866,0.403498012513773));
#12757=CARTESIAN_POINT('Ctrl Pts',(12.6,1.92335674041114,0.201930996640285));
#12758=CARTESIAN_POINT('Ctrl Pts',(12.6,1.92814168252712,0.100965094925255));
#12759=CARTESIAN_POINT('Ctrl Pts',(12.6,1.93292824674167,0.));
#12760=CARTESIAN_POINT('',(12.6,1.80383022254432,0.7));
#12761=CARTESIAN_POINT('Ctrl Pts',(12.6,1.80383022254432,0.7));
#12762=CARTESIAN_POINT('Ctrl Pts',(12.6,1.81177675668304,0.7));
#12763=CARTESIAN_POINT('Ctrl Pts',(12.6000021803669,1.81966206665253,0.699006623620781));
#12764=CARTESIAN_POINT('Ctrl Pts',(12.6000040789681,1.8273451885609,0.69711902809518));
#12765=CARTESIAN_POINT('Ctrl Pts',(12.6000050614635,1.8313210797205,0.696142227980247));
#12766=CARTESIAN_POINT('Ctrl Pts',(12.6000059683507,1.83524283435206,0.694925046992878));
#12767=CARTESIAN_POINT('Ctrl Pts',(12.6000066021136,1.83908960013903,0.693475985595303));
#12768=CARTESIAN_POINT('Ctrl Pts',(12.6000078338507,1.84656590463324,0.690659691378536));
#12769=CARTESIAN_POINT('Ctrl Pts',(12.6000078244032,1.85367932786264,0.687000939374075));
#12770=CARTESIAN_POINT('Ctrl Pts',(12.6000065509639,1.86028396908448,0.682580904467878));
#12771=CARTESIAN_POINT('Ctrl Pts',(12.600005740321,1.86448833536622,0.679767209507086));
#12772=CARTESIAN_POINT('Ctrl Pts',(12.6000044390918,1.86848632867783,0.676643963831362));
#12773=CARTESIAN_POINT('Ctrl Pts',(12.6000033339006,1.8722338275817,0.673223162566374));
#12774=CARTESIAN_POINT('Ctrl Pts',(12.6000024442799,1.87525036668517,0.670469597843409));
#12775=CARTESIAN_POINT('Ctrl Pts',(12.600001679327,1.8780865799519,0.667539409933064));
#12776=CARTESIAN_POINT('Ctrl Pts',(12.600001676908,1.88072259809992,0.664442334323256));
#12777=CARTESIAN_POINT('Ctrl Pts',(12.6000016722164,1.88583495965423,0.658435786041233));
#12778=CARTESIAN_POINT('Ctrl Pts',(12.6000042182276,1.89019731592974,0.651802923597933));
#12779=CARTESIAN_POINT('Ctrl Pts',(12.6000050838539,1.89374834224248,0.644708005294394));
#12780=CARTESIAN_POINT('Ctrl Pts',(12.60000518898,1.89417959722901,0.643846361750254));
#12781=CARTESIAN_POINT('Ctrl Pts',(12.6000052753339,1.8945988291305,0.642977876839351));
#12782=CARTESIAN_POINT('Ctrl Pts',(12.6000053405091,1.89500587920016,0.642102827114796));
#12783=CARTESIAN_POINT('Ctrl Pts',(12.6000058761205,1.89835102950234,0.634911640898031));
#12784=CARTESIAN_POINT('Ctrl Pts',(12.6000044960414,1.90083797337412,0.627363460372113));
#12785=CARTESIAN_POINT('Ctrl Pts',(12.6000025707297,1.90241244660326,0.619625605651968));
#12786=CARTESIAN_POINT('Ctrl Pts',(12.6000013488022,1.90341170938816,0.614714661398562));
#12787=CARTESIAN_POINT('Ctrl Pts',(12.5999999979477,1.90404256918024,0.609726685483646));
#12788=CARTESIAN_POINT('Ctrl Pts',(12.6000000000242,1.90428042250026,0.604702508168697));
#12789=CARTESIAN_POINT('',(12.6,-1.8038302225439,0.7));
#12790=CARTESIAN_POINT('',(12.6,-0.996884774049031,0.7));
#12791=CARTESIAN_POINT('Ctrl Pts',(12.6000000000242,-1.90428042250026,0.604702508168697));
#12792=CARTESIAN_POINT('Ctrl Pts',(12.5999999967566,-1.90390613686288,0.612608546261599));
#12793=CARTESIAN_POINT('Ctrl Pts',(12.6000030637542,-1.90256112855112,0.620429349781532));
#12794=CARTESIAN_POINT('Ctrl Pts',(12.6000044618611,-1.90032851942705,0.628004813168584));
#12795=CARTESIAN_POINT('Ctrl Pts',(12.6000051410147,-1.89924399238468,0.63168472059761));
#12796=CARTESIAN_POINT('Ctrl Pts',(12.6000055125137,-1.89794920179963,0.635306724151721));
#12797=CARTESIAN_POINT('Ctrl Pts',(12.6000054780251,-1.8964494555225,0.638851301608537));
#12798=CARTESIAN_POINT('Ctrl Pts',(12.6000054068101,-1.89335265044601,0.64617044994032));
#12799=CARTESIAN_POINT('Ctrl Pts',(12.6000033360581,-1.88942004582711,0.653077891556402));
#12800=CARTESIAN_POINT('Ctrl Pts',(12.6000021947065,-1.88472046879005,0.659412676045522));
#12801=CARTESIAN_POINT('Ctrl Pts',(12.6000018847951,-1.88344439178375,0.661132761228218));
#12802=CARTESIAN_POINT('Ctrl Pts',(12.6000016718208,-1.88211149822114,0.662810505670431));
#12803=CARTESIAN_POINT('Ctrl Pts',(12.6000016744967,-1.88072259784382,0.664442334323417));
#12804=CARTESIAN_POINT('Ctrl Pts',(12.6000016781594,-1.87882150924004,0.666675936463772));
#12805=CARTESIAN_POINT('Ctrl Pts',(12.6000020841502,-1.87681550570489,0.668823545630641));
#12806=CARTESIAN_POINT('Ctrl Pts',(12.6000026366798,-1.87471194035196,0.670881441794774));
#12807=CARTESIAN_POINT('Ctrl Pts',(12.6000041308351,-1.86902346102148,0.676446422116204));
#12808=CARTESIAN_POINT('Ctrl Pts',(12.600006461375,-1.86269053299793,0.681293522350018));
#12809=CARTESIAN_POINT('Ctrl Pts',(12.6000072160154,-1.85587841208407,0.685370830723365));
#12810=CARTESIAN_POINT('Ctrl Pts',(12.6000077023835,-1.85148797774957,0.687998669380522));
#12811=CARTESIAN_POINT('Ctrl Pts',(12.6000076405209,-1.84689749427555,0.690306084934615));
#12812=CARTESIAN_POINT('Ctrl Pts',(12.6000070464578,-1.84214500723865,0.692269637845719));
#12813=CARTESIAN_POINT('Ctrl Pts',(12.6000061272438,-1.8347913233911,0.69530790964196));
#12814=CARTESIAN_POINT('Ctrl Pts',(12.6000039197963,-1.82713360831075,0.697490862850871));
#12815=CARTESIAN_POINT('Ctrl Pts',(12.6000021173902,-1.81932000848244,0.698749700991972));
#12816=CARTESIAN_POINT('Ctrl Pts',(12.6000009388424,-1.81421089282246,0.699572823470905));
#12817=CARTESIAN_POINT('Ctrl Pts',(12.6,-1.80903450780073,0.7));
#12818=CARTESIAN_POINT('Ctrl Pts',(12.6,-1.80383022254432,0.7));
#12819=CARTESIAN_POINT('Ctrl Pts',(12.4277899437912,-1.91498765980368,8.1061082099175E-6));
#12820=CARTESIAN_POINT('Ctrl Pts',(12.4185093097394,-1.90440735427916,0.201956437811591));
#12821=CARTESIAN_POINT('Ctrl Pts',(12.4092288296506,-1.89382707230216,0.403904777849331));
#12822=CARTESIAN_POINT('Ctrl Pts',(12.3999485057213,-1.88324681432718,0.605853126346544));
#12823=CARTESIAN_POINT('Ctrl Pts',(11.2514531524596,-1.79377193015415,-0.000335869645892519));
#12824=CARTESIAN_POINT('Ctrl Pts',(11.2440495594319,-1.78319067664719,0.201611894978303));
#12825=CARTESIAN_POINT('Ctrl Pts',(11.2366461029568,-1.77260943823668,0.403559665746509));
#12826=CARTESIAN_POINT('Ctrl Pts',(11.2292427771396,-1.76202821861547,0.605507441576721));
#12827=CARTESIAN_POINT('Ctrl Pts',(10.0755218259154,-1.69940246002113,-0.00057195363688788));
#12828=CARTESIAN_POINT('Ctrl Pts',(10.0699958446785,-1.68882059084335,0.201375418496625));
#12829=CARTESIAN_POINT('Ctrl Pts',(10.0644699805481,-1.67823873210945,0.403322794723726));
#12830=CARTESIAN_POINT('Ctrl Pts',(10.0589442279885,-1.66765688783508,0.605270174140068));
#12831=CARTESIAN_POINT('Ctrl Pts',(8.90001330805802,-1.62424530699552,-0.000736768987564917));
#12832=CARTESIAN_POINT('Ctrl Pts',(8.89636559238287,-1.61366301035882,0.201210329036737));
#12833=CARTESIAN_POINT('Ctrl Pts',(8.89271797406169,-1.60308072296431,0.403157429313698));
#12834=CARTESIAN_POINT('Ctrl Pts',(8.88907045450167,-1.59249844499155,0.605104531878289));
#12835=CARTESIAN_POINT('Ctrl Pts',(8.9000000009702,-1.5932011715731,0.605106081469384));
#12836=CARTESIAN_POINT('Ctrl Pts',(10.0684994345535,-1.66840362346204,0.605023135335662));
#12837=CARTESIAN_POINT('Ctrl Pts',(11.2356615742313,-1.76272273105624,0.604904457271936));
#12838=CARTESIAN_POINT('Ctrl Pts',(12.4,-1.8833055216247,0.604732563714112));
#12839=CARTESIAN_POINT('Ctrl Pts',(12.8889963716306,-1.96391015057091,2.25514051876985E-16));
#12840=CARTESIAN_POINT('Ctrl Pts',(12.8789974396847,-1.95334878321431,0.201594505485581));
#12841=CARTESIAN_POINT('Ctrl Pts',(12.8689986695879,-1.94278744208821,0.403189020401051));
#12842=CARTESIAN_POINT('Ctrl Pts',(12.8590000636394,-1.93222612769726,0.604783544887274));
#12843=CARTESIAN_POINT('Ctrl Pts',(12.792662965057,-1.95339909479377,-3.05216148415599E-5));
#12844=CARTESIAN_POINT('Ctrl Pts',(12.7828174539371,-1.94283764251598,0.201563933758495));
#12845=CARTESIAN_POINT('Ctrl Pts',(12.7729721028852,-1.93227621586528,0.403158398317997));
#12846=CARTESIAN_POINT('Ctrl Pts',(12.7631269141758,-1.92171481533493,0.604752872200892));
#12847=CARTESIAN_POINT('Ctrl Pts',(12.6963322449993,-1.94307475200589,-6.02899321993968E-5));
#12848=CARTESIAN_POINT('Ctrl Pts',(12.6866401583647,-1.93251321719056,0.201534116532542));
#12849=CARTESIAN_POINT('Ctrl Pts',(12.6769482300299,-1.92195170741534,0.403128531945268));
#12850=CARTESIAN_POINT('Ctrl Pts',(12.6672564622455,-1.91139022316239,0.604722956439736));
#12851=CARTESIAN_POINT('Ctrl Pts',(12.6000042264769,-1.9329329264796,-8.93242901516475E-5));
#12852=CARTESIAN_POINT('Ctrl Pts',(12.5904655680581,-1.92237131142302,0.201505034443145));
#12853=CARTESIAN_POINT('Ctrl Pts',(12.5809270661843,-1.91180972083551,0.403099401891705));
#12854=CARTESIAN_POINT('Ctrl Pts',(12.5713887230828,-1.90124815518829,0.604693778185974));
#12855=CARTESIAN_POINT('',(12.8572578715866,-1.93204080633595,0.60466226999893));
#12856=CARTESIAN_POINT('Ctrl Pts',(12.6000000000242,-1.90428042250026,0.604702508168697));
#12857=CARTESIAN_POINT('Ctrl Pts',(12.6857696261193,-1.91338852735451,0.604689390578107));
#12858=CARTESIAN_POINT('Ctrl Pts',(12.7715225733429,-1.92264108900731,0.604675979983877));
#12859=CARTESIAN_POINT('Ctrl Pts',(12.8572578715866,-1.93204080633595,0.60466226999893));
#12860=CARTESIAN_POINT('Ctrl Pts',(12.8572578715866,-1.93204080633595,0.604662269998931));
#12861=CARTESIAN_POINT('Ctrl Pts',(12.867837444884,-1.94266422047353,0.403108198925376));
#12862=CARTESIAN_POINT('Ctrl Pts',(12.8784169445746,-1.95328733374019,0.201554108835025));
#12863=CARTESIAN_POINT('Ctrl Pts',(12.8889963716306,-1.96391015057091,-1.13624387676481E-16));
#12864=CARTESIAN_POINT('Ctrl Pts',(12.4102890066107,-1.7839488953552,0.7));
#12865=CARTESIAN_POINT('Ctrl Pts',(11.2423261062923,-1.6629989551888,0.7));
#12866=CARTESIAN_POINT('Ctrl Pts',(10.0717272052363,-1.56846077660453,0.7));
#12867=CARTESIAN_POINT('Ctrl Pts',(8.89999999999993,-1.49312521822106,0.7));
#12868=CARTESIAN_POINT('Ctrl Pts',(12.4072999778185,-1.81281269415102,0.7));
#12869=CARTESIAN_POINT('Ctrl Pts',(11.2397765858669,-1.69187462084457,0.699998757165067));
#12870=CARTESIAN_POINT('Ctrl Pts',(10.0695527221263,-1.59734372851255,0.700000594792869));
#12871=CARTESIAN_POINT('Ctrl Pts',(8.89814271406455,-1.52201240649035,0.7));
#12872=CARTESIAN_POINT('Ctrl Pts',(12.4021203845267,-1.86282985658401,0.676448561733929));
#12873=CARTESIAN_POINT('Ctrl Pts',(11.2353531757414,-1.74191593276004,0.676505236381959));
#12874=CARTESIAN_POINT('Ctrl Pts',(10.0657879841113,-1.64739716848489,0.676543604639643));
#12875=CARTESIAN_POINT('Ctrl Pts',(8.89492397206972,-1.57207492202614,0.676570833338327));
#12876=CARTESIAN_POINT('Ctrl Pts',(12.400106093269,-1.88228102337346,0.626471792264191));
#12877=CARTESIAN_POINT('Ctrl Pts',(11.2336287644773,-1.76143987438699,0.626617923584012));
#12878=CARTESIAN_POINT('Ctrl Pts',(10.0643137348541,-1.66697079985262,0.626717999675944));
#12879=CARTESIAN_POINT('Ctrl Pts',(8.89366330605793,-1.59168261717615,0.626788336025017));
#12880=CARTESIAN_POINT('Ctrl Pts',(12.4,-1.8833055216247,0.604732563714112));
#12881=CARTESIAN_POINT('Ctrl Pts',(11.2335332423564,-1.7625023138725,0.604904771481731));
#12882=CARTESIAN_POINT('Ctrl Pts',(10.0642324382527,-1.66805889332185,0.605023569028795));
#12883=CARTESIAN_POINT('Ctrl Pts',(8.89359217382714,-1.59278896817116,0.605106535971077));
#12884=CARTESIAN_POINT('Ctrl Pts',(12.400000003046,-1.78288409409898,0.7));
#12885=CARTESIAN_POINT('Ctrl Pts',(11.235451325406,-1.66244391065713,0.7));
#12886=CARTESIAN_POINT('Ctrl Pts',(10.0682865064676,-1.56823955876321,0.7));
#12887=CARTESIAN_POINT('Ctrl Pts',(8.89999999999993,-1.49312521822106,0.7));
#12888=CARTESIAN_POINT('Ctrl Pts',(12.8681436286308,-1.83274446434879,0.7));
#12889=CARTESIAN_POINT('Ctrl Pts',(12.7787800350189,-1.82294762441299,0.7));
#12890=CARTESIAN_POINT('Ctrl Pts',(12.6893984576578,-1.8133105623702,0.7));
#12891=CARTESIAN_POINT('Ctrl Pts',(12.6,-1.80383022254431,0.7));
#12892=CARTESIAN_POINT('Ctrl Pts',(12.8649798835675,-1.86160311979107,0.7));
#12893=CARTESIAN_POINT('Ctrl Pts',(12.7756511334299,-1.85180730951691,0.699999896874207));
#12894=CARTESIAN_POINT('Ctrl Pts',(12.686303642571,-1.84217134991284,0.700000098415946));
#12895=CARTESIAN_POINT('Ctrl Pts',(12.5969393303221,-1.83269196733649,0.7));
#12896=CARTESIAN_POINT('Ctrl Pts',(12.8594976525144,-1.91161025179704,0.676425356750174));
#12897=CARTESIAN_POINT('Ctrl Pts',(12.7702288461641,-1.90181652272411,0.676430055978541));
#12898=CARTESIAN_POINT('Ctrl Pts',(12.6809412203008,-1.89218243450198,0.676434576658958));
#12899=CARTESIAN_POINT('Ctrl Pts',(12.5916356538948,-1.88270499442535,0.67643906321291));
#12900=CARTESIAN_POINT('Ctrl Pts',(12.8573684983393,-1.93103170500986,0.626412260100396));
#12901=CARTESIAN_POINT('Ctrl Pts',(12.7681225846323,-1.92124403769089,0.626424372515079));
#12902=CARTESIAN_POINT('Ctrl Pts',(12.6788572782757,-1.91161594713487,0.626436135819418));
#12903=CARTESIAN_POINT('Ctrl Pts',(12.5895741974899,-1.90214427893475,0.626447702441804));
#12904=CARTESIAN_POINT('Ctrl Pts',(12.8572578715866,-1.93204080633595,0.60466226999893));
#12905=CARTESIAN_POINT('Ctrl Pts',(12.7680127446979,-1.92225628370762,0.604676541242762));
#12906=CARTESIAN_POINT('Ctrl Pts',(12.6787484942245,-1.91263121188365,0.60469048808123));
#12907=CARTESIAN_POINT('Ctrl Pts',(12.5894662143615,-1.9031625467727,0.604704117718382));
#12908=CARTESIAN_POINT('',(12.8681436286308,-1.83274446434879,0.7));
#12909=CARTESIAN_POINT('Ctrl Pts',(12.8681436286308,-1.83274446434879,0.7));
#12910=CARTESIAN_POINT('Ctrl Pts',(12.7787800350189,-1.82294762441299,0.7));
#12911=CARTESIAN_POINT('Ctrl Pts',(12.6893984576578,-1.8133105623702,0.7));
#12912=CARTESIAN_POINT('Ctrl Pts',(12.6,-1.80383022254431,0.7));
#12913=CARTESIAN_POINT('Origin',(12.8681436286308,-1.83274446434879,0.6));
#12914=CARTESIAN_POINT('Origin',(6.87409734069396,-2.22251806091942E-16,
0.7));
#12915=CARTESIAN_POINT('Ctrl Pts',(8.9,1.49312521822106,0.7));
#12916=CARTESIAN_POINT('Ctrl Pts',(10.0682865064677,1.56823955876321,0.7));
#12917=CARTESIAN_POINT('Ctrl Pts',(11.2354513254061,1.66244391065714,0.7));
#12918=CARTESIAN_POINT('Ctrl Pts',(12.4000000030461,1.78288409409899,0.7));
#12919=CARTESIAN_POINT('Origin',(6.87409734069396,-2.22251806091942E-16,
0.7));
#12920=CARTESIAN_POINT('',(12.8681436286308,1.83274446434879,0.7));
#12921=CARTESIAN_POINT('Ctrl Pts',(12.6,1.80383022254432,0.7));
#12922=CARTESIAN_POINT('Ctrl Pts',(12.6893984576578,1.8133105623702,0.7));
#12923=CARTESIAN_POINT('Ctrl Pts',(12.7787800350189,1.82294762441299,0.7));
#12924=CARTESIAN_POINT('Ctrl Pts',(12.8681436286308,1.83274446434879,0.7));
#12925=CARTESIAN_POINT('',(12.8681436286308,1.1,0.7));
#12926=CARTESIAN_POINT('Ctrl Pts',(8.9,1.49312521822106,0.7));
#12927=CARTESIAN_POINT('Ctrl Pts',(10.0717272052363,1.56846077660453,0.7));
#12928=CARTESIAN_POINT('Ctrl Pts',(11.2423261062923,1.6629989551888,0.7));
#12929=CARTESIAN_POINT('Ctrl Pts',(12.4102890066107,1.7839488953552,0.7));
#12930=CARTESIAN_POINT('Ctrl Pts',(8.89814271406461,1.52201240649035,0.7));
#12931=CARTESIAN_POINT('Ctrl Pts',(10.0695527221263,1.59734372851256,0.700000594792869));
#12932=CARTESIAN_POINT('Ctrl Pts',(11.2397765858669,1.69187462084457,0.699998757165067));
#12933=CARTESIAN_POINT('Ctrl Pts',(12.4072999778185,1.81281269415102,0.7));
#12934=CARTESIAN_POINT('Ctrl Pts',(8.89492397206979,1.57207492202615,0.676570833338327));
#12935=CARTESIAN_POINT('Ctrl Pts',(10.0657879841114,1.64739716848489,0.676543604639644));
#12936=CARTESIAN_POINT('Ctrl Pts',(11.2353531757414,1.74191593276004,0.676505236381959));
#12937=CARTESIAN_POINT('Ctrl Pts',(12.4021203845267,1.86282985658401,0.676448561733929));
#12938=CARTESIAN_POINT('Ctrl Pts',(8.89366330605799,1.59168261717616,0.626788336025017));
#12939=CARTESIAN_POINT('Ctrl Pts',(10.0643137348542,1.66697079985262,0.626717999675944));
#12940=CARTESIAN_POINT('Ctrl Pts',(11.2336287644773,1.761439874387,0.626617923584012));
#12941=CARTESIAN_POINT('Ctrl Pts',(12.400106093269,1.88228102337346,0.626471792264191));
#12942=CARTESIAN_POINT('Ctrl Pts',(8.89359217382721,1.59278896817116,0.605106535971077));
#12943=CARTESIAN_POINT('Ctrl Pts',(10.0642324382527,1.66805889332185,0.605023569028795));
#12944=CARTESIAN_POINT('Ctrl Pts',(11.2335332423565,1.7625023138725,0.604904771481731));
#12945=CARTESIAN_POINT('Ctrl Pts',(12.4,1.8833055216247,0.604732563714112));
#12946=CARTESIAN_POINT('Ctrl Pts',(12.4,1.8833055216247,0.604732563714112));
#12947=CARTESIAN_POINT('Ctrl Pts',(11.2356615742313,1.76272273105624,0.604904457271936));
#12948=CARTESIAN_POINT('Ctrl Pts',(10.0684994345535,1.66840362346204,0.605023135335662));
#12949=CARTESIAN_POINT('Ctrl Pts',(8.90000000097019,1.5932011715731,0.605106081469384));
#12950=CARTESIAN_POINT('Ctrl Pts',(8.90001330805765,1.62424530699444,-0.000736768966955875));
#12951=CARTESIAN_POINT('Ctrl Pts',(8.89636559238262,1.6136630103581,0.201210329050476));
#12952=CARTESIAN_POINT('Ctrl Pts',(8.89271797406156,1.60308072296395,0.403157429320568));
#12953=CARTESIAN_POINT('Ctrl Pts',(8.88907045450167,1.59249844499155,0.605104531878289));
#12954=CARTESIAN_POINT('Ctrl Pts',(10.0755218259151,1.69940246002007,-0.000571953616278766));
#12955=CARTESIAN_POINT('Ctrl Pts',(10.0699958446785,1.68882059084265,0.201375418510364));
#12956=CARTESIAN_POINT('Ctrl Pts',(10.0644699805483,1.67823873210911,0.403322794730596));
#12957=CARTESIAN_POINT('Ctrl Pts',(10.0589442279888,1.6676568878351,0.605270174140069));
#12958=CARTESIAN_POINT('Ctrl Pts',(11.2514531524595,1.79377193015312,-0.000335869625283423));
#12959=CARTESIAN_POINT('Ctrl Pts',(11.244049559432,1.78319067664652,0.201611894992042));
#12960=CARTESIAN_POINT('Ctrl Pts',(11.2366461029572,1.77260943823637,0.403559665753379));
#12961=CARTESIAN_POINT('Ctrl Pts',(11.2292427771402,1.76202821861552,0.605507441576721));
#12962=CARTESIAN_POINT('Ctrl Pts',(12.4277899437912,1.9149876598027,8.10612881915578E-6));
#12963=CARTESIAN_POINT('Ctrl Pts',(12.4185093097397,1.90440735427854,0.201956437825331));
#12964=CARTESIAN_POINT('Ctrl Pts',(12.4092288296513,1.89382707230189,0.403904777856201));
#12965=CARTESIAN_POINT('Ctrl Pts',(12.3999485057223,1.88324681432728,0.605853126346545));
#12966=CARTESIAN_POINT('Ctrl Pts',(12.6000042264759,1.9329329264795,-8.93242901520291E-5));
#12967=CARTESIAN_POINT('Ctrl Pts',(12.5904655680574,1.92237131142328,0.201505034436202));
#12968=CARTESIAN_POINT('Ctrl Pts',(12.580927066184,1.91180972083614,0.403099401877819));
#12969=CARTESIAN_POINT('Ctrl Pts',(12.5713887230828,1.90124815518927,0.604693778165146));
#12970=CARTESIAN_POINT('Ctrl Pts',(12.6963322449987,1.94307475200582,-6.02899321996874E-5));
#12971=CARTESIAN_POINT('Ctrl Pts',(12.6866401583644,1.93251321719085,0.201534116525599));
#12972=CARTESIAN_POINT('Ctrl Pts',(12.6769482300299,1.921951707416,0.403128531931383));
#12973=CARTESIAN_POINT('Ctrl Pts',(12.6672564622458,1.91139022316341,0.604722956418908));
#12974=CARTESIAN_POINT('Ctrl Pts',(12.7926629650567,1.95339909479374,-3.05216148420481E-5));
#12975=CARTESIAN_POINT('Ctrl Pts',(12.7828174539371,1.94283764251631,0.201563933751552));
#12976=CARTESIAN_POINT('Ctrl Pts',(12.7729721028855,1.93227621586597,0.403158398304112));
#12977=CARTESIAN_POINT('Ctrl Pts',(12.7631269141765,1.92171481533599,0.604752872180064));
#12978=CARTESIAN_POINT('Ctrl Pts',(12.8889963716306,1.96391015057091,-1.66533453693773E-16));
#12979=CARTESIAN_POINT('Ctrl Pts',(12.878997439685,1.95334878321468,0.201594505478638));
#12980=CARTESIAN_POINT('Ctrl Pts',(12.8689986695886,1.94278744208894,0.403189020387166));
#12981=CARTESIAN_POINT('Ctrl Pts',(12.8590000636404,1.93222612769835,0.604783544866446));
#12982=CARTESIAN_POINT('',(12.8572578715866,1.93204080633595,0.60466226999893));
#12983=CARTESIAN_POINT('Ctrl Pts',(12.8889963716306,1.96391015057091,-3.88144377749811E-17));
#12984=CARTESIAN_POINT('Ctrl Pts',(12.8784169445746,1.95328733374019,0.201554108835021));
#12985=CARTESIAN_POINT('Ctrl Pts',(12.867837444884,1.94266422047353,0.403108198925375));
#12986=CARTESIAN_POINT('Ctrl Pts',(12.8572578715866,1.93204080633595,0.604662269998929));
#12987=CARTESIAN_POINT('Ctrl Pts',(12.8572578715866,1.93204080633595,0.60466226999893));
#12988=CARTESIAN_POINT('Ctrl Pts',(12.7715225733429,1.92264108900731,0.604675979983877));
#12989=CARTESIAN_POINT('Ctrl Pts',(12.6857696261193,1.91338852735451,0.604689390578107));
#12990=CARTESIAN_POINT('Ctrl Pts',(12.6000000000242,1.90428042250026,0.604702508168697));
#12991=CARTESIAN_POINT('Origin',(8.7,1.68851851851852,0.));
#12992=CARTESIAN_POINT('',(8.7,-1.5805153611151,0.605119933308333));
#12993=CARTESIAN_POINT('Ctrl Pts',(8.7,-1.5805153611151,0.605119933308333));
#12994=CARTESIAN_POINT('Ctrl Pts',(8.7,-1.58569938832865,0.504197823486131));
#12995=CARTESIAN_POINT('Ctrl Pts',(8.7,-1.59088373519313,0.403275164205241));
#12996=CARTESIAN_POINT('Ctrl Pts',(8.7,-1.60124586355191,0.201568897935389));
#12997=CARTESIAN_POINT('Ctrl Pts',(8.7,-1.60642370224807,0.10078416210737));
#12998=CARTESIAN_POINT('Ctrl Pts',(8.7,-1.61160179736194,0.));
#12999=CARTESIAN_POINT('',(8.7,-1.48045180431786,0.7));
#13000=CARTESIAN_POINT('Ctrl Pts',(8.70000000036779,-1.48045180452391,0.7));
#13001=CARTESIAN_POINT('Ctrl Pts',(8.70000000202598,-1.48836706478042,0.699999999180279));
#13002=CARTESIAN_POINT('Ctrl Pts',(8.70000127066624,-1.49622113223642,0.699007614827928));
#13003=CARTESIAN_POINT('Ctrl Pts',(8.70000237141531,-1.50387364922569,0.697121884028934));
#13004=CARTESIAN_POINT('Ctrl Pts',(8.70000291188189,-1.50763102664002,0.696195992283305));
#13005=CARTESIAN_POINT('Ctrl Pts',(8.70000341240591,-1.51133980954515,0.695053883793301));
#13006=CARTESIAN_POINT('Ctrl Pts',(8.70000377175886,-1.51498230649063,0.693702880475192));
#13007=CARTESIAN_POINT('Ctrl Pts',(8.70000450976793,-1.52246296255016,0.690928302676144));
#13008=CARTESIAN_POINT('Ctrl Pts',(8.70000452394134,-1.52958344744078,0.687306123577328));
#13009=CARTESIAN_POINT('Ctrl Pts',(8.70000379461986,-1.53619834892264,0.682919715776694));
#13010=CARTESIAN_POINT('Ctrl Pts',(8.70000333219987,-1.54039247012311,0.680138551763745));
#13011=CARTESIAN_POINT('Ctrl Pts',(8.70000258238552,-1.54438316197938,0.67704909562189));
#13012=CARTESIAN_POINT('Ctrl Pts',(8.70000192913237,-1.54812716280968,0.67366362845569));
#13013=CARTESIAN_POINT('Ctrl Pts',(8.70000138361353,-1.55125370412533,0.670836491537814));
#13014=CARTESIAN_POINT('Ctrl Pts',(8.70000090341281,-1.55418891097064,0.66782012731024));
#13015=CARTESIAN_POINT('Ctrl Pts',(8.7000009033621,-1.55691103280728,0.664625500020687));
#13016=CARTESIAN_POINT('Ctrl Pts',(8.7000009032669,-1.56202159382457,0.658627848677152));
#13017=CARTESIAN_POINT('Ctrl Pts',(8.70000241148087,-1.56638404855443,0.652003279246098));
#13018=CARTESIAN_POINT('Ctrl Pts',(8.70000292788623,-1.5699383402149,0.64491699469699));
#13019=CARTESIAN_POINT('Ctrl Pts',(8.70000298354275,-1.57032141040405,0.644153257609021));
#13020=CARTESIAN_POINT('Ctrl Pts',(8.70000303046442,-1.57069504840788,0.643384135640712));
#13021=CARTESIAN_POINT('Ctrl Pts',(8.70000306761332,-1.57105914547653,0.642609822781892));
#13022=CARTESIAN_POINT('Ctrl Pts',(8.70000341208914,-1.57443535963509,0.635429742901602));
#13023=CARTESIAN_POINT('Ctrl Pts',(8.70000263566904,-1.57695592401075,0.627888404173009));
#13024=CARTESIAN_POINT('Ctrl Pts',(8.70000151703179,-1.57856725066757,0.620153930269154));
#13025=CARTESIAN_POINT('Ctrl Pts',(8.70000080174396,-1.57959757782623,0.615208292159515));
#13026=CARTESIAN_POINT('Ctrl Pts',(8.7,-1.58025528705454,0.610183028431161));
#13027=CARTESIAN_POINT('Ctrl Pts',(8.7,-1.5805153611151,0.605119933308333));
#13028=CARTESIAN_POINT('',(8.7,1.48045180431904,0.7));
#13029=CARTESIAN_POINT('',(8.7,0.844259259259259,0.7));
#13030=CARTESIAN_POINT('',(8.7,1.5805153611151,0.605119933308333));
#13031=CARTESIAN_POINT('Ctrl Pts',(8.7,1.5805153611151,0.605119933308333));
#13032=CARTESIAN_POINT('Ctrl Pts',(8.7,1.58010890623597,0.61303275518587));
#13033=CARTESIAN_POINT('Ctrl Pts',(8.70000179355525,1.57873376841273,0.620855553142259));
#13034=CARTESIAN_POINT('Ctrl Pts',(8.7000025961206,1.5764741717406,0.62842799710221));
#13035=CARTESIAN_POINT('Ctrl Pts',(8.70000304562639,1.57520860278123,0.632669218617747));
#13036=CARTESIAN_POINT('Ctrl Pts',(8.70000324668712,1.57366457852079,0.636831947144834));
#13037=CARTESIAN_POINT('Ctrl Pts',(8.70000313318341,1.57185009366145,0.640886032861668));
#13038=CARTESIAN_POINT('Ctrl Pts',(8.70000293045856,1.56860930815545,0.648126888117959));
#13039=CARTESIAN_POINT('Ctrl Pts',(8.70000158438082,1.56454425420738,0.654942317779106));
#13040=CARTESIAN_POINT('Ctrl Pts',(8.70000106269264,1.55971945710293,0.661169479919421));
#13041=CARTESIAN_POINT('Ctrl Pts',(8.70000096439252,1.55881033523018,0.662342845179011));
#13042=CARTESIAN_POINT('Ctrl Pts',(8.70000090351839,1.55787410801649,0.663495254390581));
#13043=CARTESIAN_POINT('Ctrl Pts',(8.70000090409683,1.55691103285321,0.664625500020665));
#13044=CARTESIAN_POINT('Ctrl Pts',(8.70000090523835,1.55501044337284,0.666855993586132));
#13045=CARTESIAN_POINT('Ctrl Pts',(8.70000114361209,1.55300532702719,0.669000219206223));
#13046=CARTESIAN_POINT('Ctrl Pts',(8.70000146777886,1.55090303951829,0.671054438207787));
#13047=CARTESIAN_POINT('Ctrl Pts',(8.70000234447876,1.54521746205001,0.676610015749294));
#13048=CARTESIAN_POINT('Ctrl Pts',(8.70000370702799,1.53888821826629,0.681447385411957));
#13049=CARTESIAN_POINT('Ctrl Pts',(8.70000415375638,1.53207947242364,0.685512859850771));
#13050=CARTESIAN_POINT('Ctrl Pts',(8.70000443876751,1.52773551673798,0.688106618115728));
#13051=CARTESIAN_POINT('Ctrl Pts',(8.70000441165582,1.52319541573235,0.690385508075002));
#13052=CARTESIAN_POINT('Ctrl Pts',(8.70000407315693,1.51849599021366,0.692326230693156));
#13053=CARTESIAN_POINT('Ctrl Pts',(8.70000354533424,1.51116815716702,0.695352407250086));
#13054=CARTESIAN_POINT('Ctrl Pts',(8.70000225790696,1.50353761203248,0.697524030080351));
#13055=CARTESIAN_POINT('Ctrl Pts',(8.70000121423997,1.49575164755759,0.698771658000832));
#13056=CARTESIAN_POINT('Ctrl Pts',(8.70000053774506,1.49070486028667,0.699580358416591));
#13057=CARTESIAN_POINT('Ctrl Pts',(8.70000000144466,1.48559217323052,0.699999999467653));
#13058=CARTESIAN_POINT('Ctrl Pts',(8.70000000036779,1.48045180452391,0.7));
#13059=CARTESIAN_POINT('Ctrl Pts',(8.7,1.61160179736194,0.));
#13060=CARTESIAN_POINT('Ctrl Pts',(8.7,1.60642368739695,0.100784451162898));
#13061=CARTESIAN_POINT('Ctrl Pts',(8.7,1.60124583384883,0.201569476094892));
#13062=CARTESIAN_POINT('Ctrl Pts',(8.7,1.59088370548997,0.403275742430776));
#13063=CARTESIAN_POINT('Ctrl Pts',(8.7,1.58569937347746,0.504198112607714));
#13064=CARTESIAN_POINT('Ctrl Pts',(8.7,1.5805153611151,0.605119933308333));
#13065=CARTESIAN_POINT('Ctrl Pts',(8.7100201910492,-1.61222456240079,1.33887903992595E-6));
#13066=CARTESIAN_POINT('Ctrl Pts',(8.70667727354472,-1.60164608969543,0.201874135619687));
#13067=CARTESIAN_POINT('Ctrl Pts',(8.70333445073708,-1.59106762573893,0.40374693439627));
#13068=CARTESIAN_POINT('Ctrl Pts',(8.69999172399519,-1.58048917070122,0.605619735240497));
#13069=CARTESIAN_POINT('Ctrl Pts',(7.30266630830786,-1.52469223633113,-0.000186944012493601));
#13070=CARTESIAN_POINT('Ctrl Pts',(7.3015714609838,-1.51411327886182,0.201685539385837));
#13071=CARTESIAN_POINT('Ctrl Pts',(7.30047669312962,-1.50353432123569,0.403558023359813));
#13072=CARTESIAN_POINT('Ctrl Pts',(7.2993819983171,-1.49295537435081,0.605430507723141));
#13073=CARTESIAN_POINT('Ctrl Pts',(5.89591889571946,-1.46411055243784,-0.000276130330627546));
#13074=CARTESIAN_POINT('Ctrl Pts',(5.8970730573458,-1.45353136553189,0.201596203763285));
#13075=CARTESIAN_POINT('Ctrl Pts',(5.89822728315403,-1.44295217665945,0.403468537584815));
#13076=CARTESIAN_POINT('Ctrl Pts',(5.89938156763751,-1.43237299696387,0.60534087113472));
#13077=CARTESIAN_POINT('Ctrl Pts',(4.48978738186403,-1.41740792524342,-0.000330195618103912));
#13078=CARTESIAN_POINT('Ctrl Pts',(4.49319153668887,-1.4068286019831,0.201542048187911));
#13079=CARTESIAN_POINT('Ctrl Pts',(4.49659574248722,-1.39624928130228,0.403414291272231));
#13080=CARTESIAN_POINT('Ctrl Pts',(4.5,-1.3856699632509,0.605286533625018));
#13081=CARTESIAN_POINT('Ctrl Pts',(4.50000000014037,-1.38566996330298,0.605286533623957));
#13082=CARTESIAN_POINT('Ctrl Pts',(5.90109530155974,-1.43243455365708,0.605259331490037));
#13083=CARTESIAN_POINT('Ctrl Pts',(7.30150776148394,-1.49309969195427,0.605214402664297));
#13084=CARTESIAN_POINT('Ctrl Pts',(8.7,-1.5805153611151,0.605119933308333));
#13085=CARTESIAN_POINT('Ctrl Pts',(8.7062300060629,-1.48084102486261,0.7));
#13086=CARTESIAN_POINT('Ctrl Pts',(7.30535837857749,-1.39328148786737,0.7));
#13087=CARTESIAN_POINT('Ctrl Pts',(5.90286553803659,-1.3325543763676,0.7));
#13088=CARTESIAN_POINT('Ctrl Pts',(4.5,-1.28575421950843,0.7));
#13089=CARTESIAN_POINT('Ctrl Pts',(8.7044244076592,-1.50972892972339,0.7));
#13090=CARTESIAN_POINT('Ctrl Pts',(7.30392377861185,-1.42217417124324,0.699999322371676));
#13091=CARTESIAN_POINT('Ctrl Pts',(5.90170976758769,-1.36144968116949,0.700000194339816));
#13092=CARTESIAN_POINT('Ctrl Pts',(4.49903600403804,-1.314650633636,0.7));
#13093=CARTESIAN_POINT('Ctrl Pts',(8.70129509098077,-1.55979510296572,0.676577193851887));
#13094=CARTESIAN_POINT('Ctrl Pts',(7.30143307762773,-1.47225060169427,0.676608218952397));
#13095=CARTESIAN_POINT('Ctrl Pts',(5.89970879741633,-1.41153023905743,0.676622651488038));
#13096=CARTESIAN_POINT('Ctrl Pts',(4.49736521340071,-1.36473368385825,0.676631564755462));
#13097=CARTESIAN_POINT('Ctrl Pts',(8.70006933407556,-1.57940608001781,0.626799670546273));
#13098=CARTESIAN_POINT('Ctrl Pts',(7.3004573192207,-1.49190036240803,0.626879818917698));
#13099=CARTESIAN_POINT('Ctrl Pts',(5.89892183391985,-1.43119871194172,0.62691759730524));
#13100=CARTESIAN_POINT('Ctrl Pts',(4.49670869913724,-1.38441313147668,0.626940642142451));
#13101=CARTESIAN_POINT('Ctrl Pts',(8.7,-1.5805153611151,0.605119933308333));
#13102=CARTESIAN_POINT('Ctrl Pts',(7.30039998287682,-1.49303044794594,0.605214477495697));
#13103=CARTESIAN_POINT('Ctrl Pts',(5.89887670103551,-1.4323384618751,0.605259402637312));
#13104=CARTESIAN_POINT('Ctrl Pts',(4.49667047719213,-1.38555885946567,0.605286598232956));
#13105=CARTESIAN_POINT('Ctrl Pts',(8.70000000036771,-1.48045180452391,0.7));
#13106=CARTESIAN_POINT('Ctrl Pts',(7.30120024114866,-1.39310147361351,0.7));
#13107=CARTESIAN_POINT('Ctrl Pts',(5.90078591724148,-1.332484999384,0.7));
#13108=CARTESIAN_POINT('Ctrl Pts',(4.5,-1.28575421950843,0.7));
#13109=CARTESIAN_POINT('Origin',(6.87409734069396,-2.22251806091942E-16,
0.7));
#13110=CARTESIAN_POINT('Ctrl Pts',(4.5,1.28575421950843,0.7));
#13111=CARTESIAN_POINT('Ctrl Pts',(5.9007859172415,1.332484999384,0.7));
#13112=CARTESIAN_POINT('Ctrl Pts',(7.30120024114871,1.39310147361351,0.7));
#13113=CARTESIAN_POINT('Ctrl Pts',(8.70000000036779,1.48045180452391,0.7));
#13114=CARTESIAN_POINT('Ctrl Pts',(4.5,1.28575421950843,0.7));
#13115=CARTESIAN_POINT('Ctrl Pts',(5.90286553803659,1.3325543763676,0.7));
#13116=CARTESIAN_POINT('Ctrl Pts',(7.30535837857749,1.39328148786737,0.7));
#13117=CARTESIAN_POINT('Ctrl Pts',(8.7062300060629,1.48084102486261,0.7));
#13118=CARTESIAN_POINT('Ctrl Pts',(4.49903600403804,1.314650633636,0.7));
#13119=CARTESIAN_POINT('Ctrl Pts',(5.90170976758769,1.36144968116949,0.700000194339816));
#13120=CARTESIAN_POINT('Ctrl Pts',(7.30392377861185,1.42217417124324,0.699999322371676));
#13121=CARTESIAN_POINT('Ctrl Pts',(8.7044244076592,1.50972892972339,0.7));
#13122=CARTESIAN_POINT('Ctrl Pts',(4.49736521340071,1.36473368385825,0.676631564755462));
#13123=CARTESIAN_POINT('Ctrl Pts',(5.89970879741633,1.41153023905743,0.676622651488038));
#13124=CARTESIAN_POINT('Ctrl Pts',(7.30143307762774,1.47225060169427,0.676608218952397));
#13125=CARTESIAN_POINT('Ctrl Pts',(8.70129509098078,1.55979510296572,0.676577193851887));
#13126=CARTESIAN_POINT('Ctrl Pts',(4.49670869913724,1.38441313147668,0.626940642142451));
#13127=CARTESIAN_POINT('Ctrl Pts',(5.89892183391985,1.43119871194172,0.626917597305239));
#13128=CARTESIAN_POINT('Ctrl Pts',(7.3004573192207,1.49190036240803,0.626879818917698));
#13129=CARTESIAN_POINT('Ctrl Pts',(8.70006933407556,1.57940608001781,0.626799670546273));
#13130=CARTESIAN_POINT('Ctrl Pts',(4.49667047719213,1.38555885946567,0.605286598232956));
#13131=CARTESIAN_POINT('Ctrl Pts',(5.89887670103551,1.4323384618751,0.605259402637312));
#13132=CARTESIAN_POINT('Ctrl Pts',(7.30039998287682,1.49303044794594,0.605214477495697));
#13133=CARTESIAN_POINT('Ctrl Pts',(8.7,1.5805153611151,0.605119933308333));
#13134=CARTESIAN_POINT('Ctrl Pts',(8.7,1.5805153611151,0.605119933308333));
#13135=CARTESIAN_POINT('Ctrl Pts',(7.30150776148394,1.49309969195427,0.605214402664297));
#13136=CARTESIAN_POINT('Ctrl Pts',(5.90109530155974,1.43243455365708,0.605259331490037));
#13137=CARTESIAN_POINT('Ctrl Pts',(4.50000000014037,1.38566996330298,0.605286533623957));
#13138=CARTESIAN_POINT('Ctrl Pts',(4.48978738186405,1.41740792524342,-0.00033019561810394));
#13139=CARTESIAN_POINT('Ctrl Pts',(4.49319153668889,1.40682860198312,0.201542048187577));
#13140=CARTESIAN_POINT('Ctrl Pts',(4.49659574248723,1.39624928130232,0.403414291271564));
#13141=CARTESIAN_POINT('Ctrl Pts',(4.5,1.38566996325095,0.605286533624017));
#13142=CARTESIAN_POINT('Ctrl Pts',(5.89591889571947,1.46411055243784,-0.000276130330627574));
#13143=CARTESIAN_POINT('Ctrl Pts',(5.89707305734581,1.45353136553191,0.201596203762952));
#13144=CARTESIAN_POINT('Ctrl Pts',(5.89822728315404,1.44295217665948,0.403468537584147));
#13145=CARTESIAN_POINT('Ctrl Pts',(5.89938156763751,1.43237299696393,0.605340871133719));
#13146=CARTESIAN_POINT('Ctrl Pts',(7.30266630830786,1.52469223633113,-0.000186944012493549));
#13147=CARTESIAN_POINT('Ctrl Pts',(7.3015714609838,1.51411327886184,0.201685539385503));
#13148=CARTESIAN_POINT('Ctrl Pts',(7.30047669312963,1.50353432123572,0.403558023359145));
#13149=CARTESIAN_POINT('Ctrl Pts',(7.29938199831711,1.49295537435086,0.60543050772214));
#13150=CARTESIAN_POINT('Ctrl Pts',(8.7100201910492,1.61222456240079,1.33887903989646E-6));
#13151=CARTESIAN_POINT('Ctrl Pts',(8.70667727354472,1.60164608969545,0.201874135619353));
#13152=CARTESIAN_POINT('Ctrl Pts',(8.7033344507371,1.59106762573896,0.403746934395602));
#13153=CARTESIAN_POINT('Ctrl Pts',(8.6999917239952,1.58048917070127,0.605619735239495));
#13154=CARTESIAN_POINT('Origin',(4.3,1.48481481481482,0.));
#13155=CARTESIAN_POINT('',(4.3,-1.37908752581626,0.605290299758539));
#13156=CARTESIAN_POINT('Ctrl Pts',(4.3,-1.37908752581626,0.605290299758539));
#13157=CARTESIAN_POINT('Ctrl Pts',(4.3,-1.38444464017247,0.504222347694443));
#13158=CARTESIAN_POINT('Ctrl Pts',(4.3,-1.38980163214303,0.403154389143214));
#13159=CARTESIAN_POINT('Ctrl Pts',(4.3,-1.40049562949383,0.201390955816302));
#13160=CARTESIAN_POINT('Ctrl Pts',(4.3,-1.40583263576898,0.100695481088992));
#13161=CARTESIAN_POINT('Ctrl Pts',(4.3,-1.41116952203211,0.));
#13162=CARTESIAN_POINT('Ctrl Pts',(4.30000000005992,-1.27917501058303,0.7));
#13163=CARTESIAN_POINT('Ctrl Pts',(4.30000000048661,-1.28708628524264,0.699999999884766));
#13164=CARTESIAN_POINT('Ctrl Pts',(4.30000064978116,-1.29493415608545,0.69900616264686));
#13165=CARTESIAN_POINT('Ctrl Pts',(4.30000121018478,-1.30257825621016,0.697119208693397));
#13166=CARTESIAN_POINT('Ctrl Pts',(4.30000152558655,-1.30688044586137,0.696057208766858));
#13167=CARTESIAN_POINT('Ctrl Pts',(4.30000181105247,-1.31111814675806,0.694711271736901));
#13168=CARTESIAN_POINT('Ctrl Pts',(4.30000199036827,-1.31526464671957,0.693092387263961));
#13169=CARTESIAN_POINT('Ctrl Pts',(4.30000231141323,-1.32268849323592,0.690193954859197));
#13170=CARTESIAN_POINT('Ctrl Pts',(4.30000222777046,-1.32973966400828,0.686455190804221));
#13171=CARTESIAN_POINT('Ctrl Pts',(4.30000179417102,-1.33627196700415,0.681957645816867));
#13172=CARTESIAN_POINT('Ctrl Pts',(4.30000155535849,-1.33986974800182,0.679480543652151));
#13173=CARTESIAN_POINT('Ctrl Pts',(4.30000121902461,-1.34330986828215,0.67677238407294));
#13174=CARTESIAN_POINT('Ctrl Pts',(4.30000092191081,-1.34656397897095,0.673841242448196));
#13175=CARTESIAN_POINT('Ctrl Pts',(4.30000063243573,-1.34973442737118,0.670985459666446));
#13176=CARTESIAN_POINT('Ctrl Pts',(4.30000037658882,-1.35270906921767,0.667935271966333));
#13177=CARTESIAN_POINT('Ctrl Pts',(4.30000037869864,-1.35546536049262,0.66470214425512));
#13178=CARTESIAN_POINT('Ctrl Pts',(4.30000038260995,-1.36057515211559,0.658708362304413));
#13179=CARTESIAN_POINT('Ctrl Pts',(4.30000117797282,-1.36493744806469,0.652087250959406));
#13180=CARTESIAN_POINT('Ctrl Pts',(4.30000145944905,-1.36849285270534,0.645004510397983));
#13181=CARTESIAN_POINT('Ctrl Pts',(4.30000148826005,-1.36885677248754,0.644279543857467));
#13182=CARTESIAN_POINT('Ctrl Pts',(4.30000151299237,-1.36921219826683,0.643549721050429));
#13183=CARTESIAN_POINT('Ctrl Pts',(4.30000153317099,-1.36955903781249,0.642815208524159));
#13184=CARTESIAN_POINT('Ctrl Pts',(4.30000173031152,-1.37294758118467,0.635639188419686));
#13185=CARTESIAN_POINT('Ctrl Pts',(4.30000134819424,-1.37548140076902,0.628100134775109));
#13186=CARTESIAN_POINT('Ctrl Pts',(4.30000077902196,-1.37710733725971,0.620366659714886));
#13187=CARTESIAN_POINT('Ctrl Pts',(4.30000041405338,-1.37814993145247,0.615407747584041));
#13188=CARTESIAN_POINT('Ctrl Pts',(4.3,-1.37881837002099,0.610368224776708));
#13189=CARTESIAN_POINT('Ctrl Pts',(4.3,-1.37908752581626,0.605290299758539));
#13190=CARTESIAN_POINT('',(4.3,1.37908752581626,0.605290299758539));
#13191=CARTESIAN_POINT('Ctrl Pts',(4.3,1.37908752581626,0.605290299758539));
#13192=CARTESIAN_POINT('Ctrl Pts',(4.3,1.37866806817032,0.613203837240499));
#13193=CARTESIAN_POINT('Ctrl Pts',(4.30000092021544,1.37728139671899,0.621026590428679));
#13194=CARTESIAN_POINT('Ctrl Pts',(4.30000132151137,1.37501133257008,0.628597948954885));
#13195=CARTESIAN_POINT('Ctrl Pts',(4.30000154544343,1.37374458621782,0.632822935636113));
#13196=CARTESIAN_POINT('Ctrl Pts',(4.30000164013187,1.37220176226583,0.636969676056352));
#13197=CARTESIAN_POINT('Ctrl Pts',(4.30000157305315,1.37039070587839,0.641008268098125));
#13198=CARTESIAN_POINT('Ctrl Pts',(4.30000145288191,1.36714620633991,0.648243387946652));
#13199=CARTESIAN_POINT('Ctrl Pts',(4.30000073948134,1.36307905360626,0.655053358422861));
#13200=CARTESIAN_POINT('Ctrl Pts',(4.3000004635866,1.35825284513469,0.661274801567968));
#13201=CARTESIAN_POINT('Ctrl Pts',(4.30000041199046,1.35735027731582,0.662438297592388));
#13202=CARTESIAN_POINT('Ctrl Pts',(4.30000037986005,1.35642103364291,0.663581140343808));
#13203=CARTESIAN_POINT('Ctrl Pts',(4.30000037943224,1.35546536051643,0.664702144255114));
#13204=CARTESIAN_POINT('Ctrl Pts',(4.300000378582,1.3535659898678,0.666930104702213));
#13205=CARTESIAN_POINT('Ctrl Pts',(4.3000005018795,1.35156225525783,0.669071850305581));
#13206=CARTESIAN_POINT('Ctrl Pts',(4.30000067038034,1.34946148384904,0.671123623013939));
#13207=CARTESIAN_POINT('Ctrl Pts',(4.30000112630012,1.34377733881547,0.676675190215126));
#13208=CARTESIAN_POINT('Ctrl Pts',(4.30000183907902,1.33744971106208,0.68150833207295));
#13209=CARTESIAN_POINT('Ctrl Pts',(4.30000208123143,1.33064243458576,0.685568782013219));
#13210=CARTESIAN_POINT('Ctrl Pts',(4.30000223513396,1.3263159977886,0.688149444058562));
#13211=CARTESIAN_POINT('Ctrl Pts',(4.3000022300233,1.32179485563522,0.690417305529342));
#13212=CARTESIAN_POINT('Ctrl Pts',(4.30000206344016,1.31711540146937,0.692349146556373));
#13213=CARTESIAN_POINT('Ctrl Pts',(4.3000018029167,1.30979708846622,0.695370400063095));
#13214=CARTESIAN_POINT('Ctrl Pts',(4.30000114702936,1.30217656646843,0.69753735975804));
#13215=CARTESIAN_POINT('Ctrl Pts',(4.3000006156201,1.29440092269557,0.69878042986007));
#13216=CARTESIAN_POINT('Ctrl Pts',(4.30000027236218,1.28937833178082,0.699583377215073));
#13217=CARTESIAN_POINT('Ctrl Pts',(4.30000000033581,1.28429042584107,0.69999999992549));
#13218=CARTESIAN_POINT('Ctrl Pts',(4.30000000005992,1.27917501058303,0.7));
#13219=CARTESIAN_POINT('Ctrl Pts',(4.3,1.41116952203211,0.));
#13220=CARTESIAN_POINT('Ctrl Pts',(4.3,1.40583262613343,0.100695662891028));
#13221=CARTESIAN_POINT('Ctrl Pts',(4.3,1.40049561022223,0.201391319421434));
#13222=CARTESIAN_POINT('Ctrl Pts',(4.3,1.38980161287056,0.403154752748307));
#13223=CARTESIAN_POINT('Ctrl Pts',(4.3,1.38444463053604,0.504222529496425));
#13224=CARTESIAN_POINT('Ctrl Pts',(4.3,1.37908752581626,0.605290299758539));
#13225=CARTESIAN_POINT('Ctrl Pts',(4.3,-1.41116952203217,-1.08233907947231E-12));
#13226=CARTESIAN_POINT('Ctrl Pts',(4.30370667985561,-1.40059355144761,0.201807922462111));
#13227=CARTESIAN_POINT('Ctrl Pts',(4.30741340932898,-1.39001758331341,0.403615844144917));
#13228=CARTESIAN_POINT('Ctrl Pts',(4.31112018914117,-1.37944161767694,0.605423765036612));
#13229=CARTESIAN_POINT('Ctrl Pts',(3.22410085073145,-1.37636920007795,-3.90459529712038E-5));
#13230=CARTESIAN_POINT('Ctrl Pts',(3.2295286994181,-1.36579313421488,0.201768811380596));
#13231=CARTESIAN_POINT('Ctrl Pts',(3.23495659078338,-1.35521706809947,0.403576667516588));
#13232=CARTESIAN_POINT('Ctrl Pts',(3.24038452463065,-1.34464100578453,0.605384522622892));
#13233=CARTESIAN_POINT('Ctrl Pts',(2.14856196511704,-1.34935185539723,-5.92140864038068E-5));
#13234=CARTESIAN_POINT('Ctrl Pts',(2.15571155670467,-1.33877574824886,0.201748609775608));
#13235=CARTESIAN_POINT('Ctrl Pts',(2.16286118630165,-1.32819964054015,0.403556432267456));
#13236=CARTESIAN_POINT('Ctrl Pts',(2.17001085376486,-1.31762353633116,0.605364253566666));
#13237=CARTESIAN_POINT('Ctrl Pts',(1.073384157387,-1.32427529283232,-8.86713468529234E-5));
#13238=CARTESIAN_POINT('Ctrl Pts',(1.08225606990756,-1.31369916974321,0.201719104822629));
#13239=CARTESIAN_POINT('Ctrl Pts',(1.09112801825726,-1.30312304798914,0.403526879488275));
#13240=CARTESIAN_POINT('Ctrl Pts',(1.10000000295732,-1.29254692759565,0.605334652628532));
#13241=CARTESIAN_POINT('Ctrl Pts',(1.10000000298281,-1.29254692760111,0.605334652628557));
#13242=CARTESIAN_POINT('Ctrl Pts',(2.16694388170712,-1.31755402957363,0.605319894542965));
#13243=CARTESIAN_POINT('Ctrl Pts',(3.23367147240841,-1.34448060345116,0.605309774863278));
#13244=CARTESIAN_POINT('Ctrl Pts',(4.3,-1.37908752581626,0.605290299758539));
#13245=CARTESIAN_POINT('Ctrl Pts',(4.30323908112369,-1.2792801058419,0.7));
#13246=CARTESIAN_POINT('Ctrl Pts',(3.23565147654712,-1.24463335454069,0.7));
#13247=CARTESIAN_POINT('Ctrl Pts',(2.1678436779024,-1.21768649131741,0.7));
#13248=CARTESIAN_POINT('Ctrl Pts',(1.09999999999999,-1.19266190204553,0.7));
#13249=CARTESIAN_POINT('Ctrl Pts',(4.30230129178181,-1.30817667592415,0.7));
#13250=CARTESIAN_POINT('Ctrl Pts',(3.23485320804887,-1.27353066282864,0.699999860738333));
#13251=CARTESIAN_POINT('Ctrl Pts',(2.16713169816659,-1.24658393122273,0.700000105496227));
#13252=CARTESIAN_POINT('Ctrl Pts',(1.0993228455422,-1.22155728565617,0.7));
#13253=CARTESIAN_POINT('Ctrl Pts',(4.30067574076257,-1.35826558912881,0.676637683834297));
#13254=CARTESIAN_POINT('Ctrl Pts',(3.23346787205668,-1.32362126434549,0.676644071225102));
#13255=CARTESIAN_POINT('Ctrl Pts',(2.16589795861771,-1.29667457247055,0.676647306834711));
#13256=CARTESIAN_POINT('Ctrl Pts',(1.09814906228501,-1.27164470234869,0.676652147774997));
#13257=CARTESIAN_POINT('Ctrl Pts',(4.30003720890047,-1.37794098943329,0.626943772371838));
#13258=CARTESIAN_POINT('Ctrl Pts',(3.23292426239396,-1.34330449078822,0.626960286972675));
#13259=CARTESIAN_POINT('Ctrl Pts',(2.16541285690349,-1.31636171257899,0.6269687859393));
#13260=CARTESIAN_POINT('Ctrl Pts',(1.09768760301306,-1.29133598921902,0.626981304916489));
#13261=CARTESIAN_POINT('Ctrl Pts',(4.3,-1.37908752581626,0.605290299758539));
#13262=CARTESIAN_POINT('Ctrl Pts',(3.23289209128077,-1.34445530919946,0.605309789097661));
#13263=CARTESIAN_POINT('Ctrl Pts',(2.16538453588699,-1.31751467232976,0.605319909330946));
#13264=CARTESIAN_POINT('Ctrl Pts',(1.09766050997011,-1.29249209748956,0.605334684996117));
#13265=CARTESIAN_POINT('Ctrl Pts',(1.09999999999999,1.19266190204553,0.7));
#13266=CARTESIAN_POINT('Ctrl Pts',(2.1678436779024,1.21768649131741,0.7));
#13267=CARTESIAN_POINT('Ctrl Pts',(3.23565147654712,1.24463335454069,0.7));
#13268=CARTESIAN_POINT('Ctrl Pts',(4.30323908112369,1.2792801058419,0.7));
#13269=CARTESIAN_POINT('Ctrl Pts',(1.0993228455422,1.22155728565617,0.7));
#13270=CARTESIAN_POINT('Ctrl Pts',(2.16713169816659,1.24658393122273,0.700000105496227));
#13271=CARTESIAN_POINT('Ctrl Pts',(3.23485320804887,1.27353066282864,0.699999860738333));
#13272=CARTESIAN_POINT('Ctrl Pts',(4.30230129178181,1.30817667592415,0.7));
#13273=CARTESIAN_POINT('Ctrl Pts',(1.09814906228501,1.27164470234869,0.676652147774997));
#13274=CARTESIAN_POINT('Ctrl Pts',(2.16589795861771,1.29667457247055,0.676647306834711));
#13275=CARTESIAN_POINT('Ctrl Pts',(3.23346787205668,1.32362126434549,0.676644071225102));
#13276=CARTESIAN_POINT('Ctrl Pts',(4.30067574076257,1.35826558912881,0.676637683834297));
#13277=CARTESIAN_POINT('Ctrl Pts',(1.09768760301306,1.29133598921902,0.626981304916489));
#13278=CARTESIAN_POINT('Ctrl Pts',(2.16541285690349,1.31636171257899,0.6269687859393));
#13279=CARTESIAN_POINT('Ctrl Pts',(3.23292426239396,1.34330449078822,0.626960286972675));
#13280=CARTESIAN_POINT('Ctrl Pts',(4.30003720890047,1.37794098943329,0.626943772371838));
#13281=CARTESIAN_POINT('Ctrl Pts',(1.09766050997011,1.29249209748956,0.605334684996117));
#13282=CARTESIAN_POINT('Ctrl Pts',(2.16538453588699,1.31751467232976,0.605319909330946));
#13283=CARTESIAN_POINT('Ctrl Pts',(3.23289209128077,1.34445530919946,0.605309789097661));
#13284=CARTESIAN_POINT('Ctrl Pts',(4.3,1.37908752581626,0.605290299758539));
#13285=CARTESIAN_POINT('Ctrl Pts',(4.3,1.37908752581626,0.605290299758539));
#13286=CARTESIAN_POINT('Ctrl Pts',(3.23367147240841,1.34448060345116,0.605309774863278));
#13287=CARTESIAN_POINT('Ctrl Pts',(2.16694388170711,1.31755402957363,0.605319894542965));
#13288=CARTESIAN_POINT('Ctrl Pts',(1.10000000298281,1.29254692760111,0.605334652628557));
#13289=CARTESIAN_POINT('Ctrl Pts',(1.07338415738705,1.32427529283227,-8.86713457716078E-5));
#13290=CARTESIAN_POINT('Ctrl Pts',(1.08225606990759,1.31369916974318,0.201719104823349));
#13291=CARTESIAN_POINT('Ctrl Pts',(1.09112801825728,1.30312304798912,0.403526879488635));
#13292=CARTESIAN_POINT('Ctrl Pts',(1.10000000295732,1.29254692759565,0.605334652628532));
#13293=CARTESIAN_POINT('Ctrl Pts',(2.14856196511707,1.34935185539717,-5.92140853224782E-5));
#13294=CARTESIAN_POINT('Ctrl Pts',(2.15571155670469,1.33877574824882,0.201748609776328));
#13295=CARTESIAN_POINT('Ctrl Pts',(2.16286118630166,1.32819964054013,0.403556432267816));
#13296=CARTESIAN_POINT('Ctrl Pts',(2.17001085376486,1.31762353633116,0.605364253566666));
#13297=CARTESIAN_POINT('Ctrl Pts',(3.22410085073147,1.37636920007789,-3.90459518899617E-5));
#13298=CARTESIAN_POINT('Ctrl Pts',(3.22952869941811,1.36579313421484,0.201768811381317));
#13299=CARTESIAN_POINT('Ctrl Pts',(3.23495659078338,1.35521706809945,0.403576667516948));
#13300=CARTESIAN_POINT('Ctrl Pts',(3.24038452463064,1.34464100578453,0.605384522622892));
#13301=CARTESIAN_POINT('Ctrl Pts',(4.3,1.41116952203211,-1.07899800205757E-15));
#13302=CARTESIAN_POINT('Ctrl Pts',(4.3037066798556,1.40059355144758,0.201807922462832));
#13303=CARTESIAN_POINT('Ctrl Pts',(4.30741340932897,1.39001758331339,0.403615844145277));
#13304=CARTESIAN_POINT('Ctrl Pts',(4.31112018914115,1.37944161767694,0.605423765036611));
#13305=CARTESIAN_POINT('Origin',(0.9,1.39290118819044,0.));
#13306=CARTESIAN_POINT('',(0.900000001878204,-1.28788040994396,0.605337476551879));
#13307=CARTESIAN_POINT('Ctrl Pts',(0.900000001878204,-1.28788040994396,
0.605337476551879));
#13308=CARTESIAN_POINT('Ctrl Pts',(0.900000001878204,-1.29328625806092,
0.504228160928694));
#13309=CARTESIAN_POINT('Ctrl Pts',(0.899999999999999,-1.29869191435855,
0.403118132397745));
#13310=CARTESIAN_POINT('Ctrl Pts',(0.899999999999999,-1.30947917558554,
0.201339438823693));
#13311=CARTESIAN_POINT('Ctrl Pts',(0.9,-1.31486085669789,0.100669384150719));
#13312=CARTESIAN_POINT('Ctrl Pts',(0.9,-1.32024227787037,0.));
#13313=CARTESIAN_POINT('',(0.9,-1.18799600975353,0.7));
#13314=CARTESIAN_POINT('Ctrl Pts',(0.900000000000324,-1.18799600975363,
0.7));
#13315=CARTESIAN_POINT('Ctrl Pts',(0.900000000063601,-1.19590581948314,
0.699999999935493));
#13316=CARTESIAN_POINT('Ctrl Pts',(0.900000451671414,-1.20375274583281,
0.699006541951706));
#13317=CARTESIAN_POINT('Ctrl Pts',(0.900000834722547,-1.21139610511184,
0.697120084132161));
#13318=CARTESIAN_POINT('Ctrl Pts',(0.900001049758257,-1.21568690349652,
0.696061072005504));
#13319=CARTESIAN_POINT('Ctrl Pts',(0.900001241882928,-1.21991360580594,
0.694719604949841));
#13320=CARTESIAN_POINT('Ctrl Pts',(0.900001357948449,-1.22404965357203,
0.693106547509926));
#13321=CARTESIAN_POINT('Ctrl Pts',(0.900001566283472,-1.23147376710855,
0.690211145364658));
#13322=CARTESIAN_POINT('Ctrl Pts',(0.900001483882417,-1.23852542365708,
0.686475281350474));
#13323=CARTESIAN_POINT('Ctrl Pts',(0.90000115772027,-1.24505817055452,0.681980323292531));
#13324=CARTESIAN_POINT('Ctrl Pts',(0.90000097852015,-1.2486473946309,0.67951070187031));
#13325=CARTESIAN_POINT('Ctrl Pts',(0.900000731874511,-1.25207971535834,
0.676811055842604));
#13326=CARTESIAN_POINT('Ctrl Pts',(0.90000051586667,-1.25532695882913,0.673889369778116));
#13327=CARTESIAN_POINT('Ctrl Pts',(0.900000304282776,-1.25850769714062,
0.671027521295527));
#13328=CARTESIAN_POINT('Ctrl Pts',(0.900000119565725,-1.26149151526032,
0.667969976014938));
#13329=CARTESIAN_POINT('Ctrl Pts',(0.900000124706954,-1.26425564062679,
0.664728268702146));
#13330=CARTESIAN_POINT('Ctrl Pts',(0.900000134210909,-1.26936533657602,
0.658735726205464));
#13331=CARTESIAN_POINT('Ctrl Pts',(0.900000724431276,-1.2737272220214,0.652115259198653));
#13332=CARTESIAN_POINT('Ctrl Pts',(0.900000949945503,-1.27728244659665,
0.645033014705304));
#13333=CARTESIAN_POINT('Ctrl Pts',(0.900000972753073,-1.27764200720725,
0.644316745985709));
#13334=CARTESIAN_POINT('Ctrl Pts',(0.900000992743332,-1.27799327761064,
0.64359573459864));
#13335=CARTESIAN_POINT('Ctrl Pts',(0.900001009576454,-1.27833616945273,
0.642870141642621));
#13336=CARTESIAN_POINT('Ctrl Pts',(0.900001176059944,-1.28172744954266,
0.635693858502874));
#13337=CARTESIAN_POINT('Ctrl Pts',(0.900000930108723,-1.28426399347052,
0.628153947608977));
#13338=CARTESIAN_POINT('Ctrl Pts',(0.900000539908504,-1.2858931319598,0.620419547606466));
#13339=CARTESIAN_POINT('Ctrl Pts',(0.900000289636433,-1.28693805157347,
0.615458750034127));
#13340=CARTESIAN_POINT('Ctrl Pts',(0.900000000000001,-1.28760881677759,
0.610417269724172));
#13341=CARTESIAN_POINT('Ctrl Pts',(0.900000000000001,-1.28788040985668,
0.605337476551933));
#13342=CARTESIAN_POINT('',(0.9,1.18799600975353,0.7));
#13343=CARTESIAN_POINT('',(0.9,0.696450594095222,0.7));
#13344=CARTESIAN_POINT('',(0.900000001878204,1.28788040994396,0.605337476551879));
#13345=CARTESIAN_POINT('Ctrl Pts',(0.900000000000001,1.28788040985668,0.605337476551933));
#13346=CARTESIAN_POINT('Ctrl Pts',(0.900000000000001,1.28745726486871,0.613251849878237));
#13347=CARTESIAN_POINT('Ctrl Pts',(0.900000641820462,1.28606767879774,0.621075732439556));
#13348=CARTESIAN_POINT('Ctrl Pts',(0.900000906166769,1.28379497466322,0.628648019961568));
#13349=CARTESIAN_POINT('Ctrl Pts',(0.900001053446495,1.2825287445946,0.632866896498568));
#13350=CARTESIAN_POINT('Ctrl Pts',(0.900001106693909,1.28098738700664,0.637007708770872));
#13351=CARTESIAN_POINT('Ctrl Pts',(0.900001044867119,1.27917862712792,0.641040603354488));
#13352=CARTESIAN_POINT('Ctrl Pts',(0.900000933962191,1.27593407274945,0.64827481168313));
#13353=CARTESIAN_POINT('Ctrl Pts',(0.900000399592996,1.27186725264719,0.655083885116145));
#13354=CARTESIAN_POINT('Ctrl Pts',(0.900000190596867,1.2670411556595,0.661303993035384));
#13355=CARTESIAN_POINT('Ctrl Pts',(0.900000151538061,1.26613921747962,0.662466454716044));
#13356=CARTESIAN_POINT('Ctrl Pts',(0.900000126821978,1.26521063179286,0.663608275427336));
#13357=CARTESIAN_POINT('Ctrl Pts',(0.900000125264574,1.26425564063975,0.664728268702142));
#13358=CARTESIAN_POINT('Ctrl Pts',(0.90000012217056,1.26235840892454,0.66695330163032));
#13359=CARTESIAN_POINT('Ctrl Pts',(0.900000209712012,1.26035699384613,0.66909223571964));
#13360=CARTESIAN_POINT('Ctrl Pts',(0.900000331194293,1.2582587086698,0.671141334714948));
#13361=CARTESIAN_POINT('Ctrl Pts',(0.900000660246931,1.25257519443757,0.676691620936499));
#13362=CARTESIAN_POINT('Ctrl Pts',(0.900001184896248,1.24624785575673,0.681523125886843));
#13363=CARTESIAN_POINT('Ctrl Pts',(0.900001377531805,1.23944073409582,0.685581770965975));
#13364=CARTESIAN_POINT('Ctrl Pts',(0.900001499905572,1.2351164383281,0.68816006802201));
#13365=CARTESIAN_POINT('Ctrl Pts',(0.900001510509735,1.23059756718463,0.690425789971136));
#13366=CARTESIAN_POINT('Ctrl Pts',(0.900001405318139,1.22592052877826,0.692355791713551));
#13367=CARTESIAN_POINT('Ctrl Pts',(0.900001240727996,1.21860250674997,0.695375607682216));
#13368=CARTESIAN_POINT('Ctrl Pts',(0.900000792095824,1.21098234272326,0.697541065921879));
#13369=CARTESIAN_POINT('Ctrl Pts',(0.900000425437202,1.20320741268883,0.698782789564668));
#13370=CARTESIAN_POINT('Ctrl Pts',(0.900000188792485,1.19818940410026,0.699584208982791));
#13371=CARTESIAN_POINT('Ctrl Pts',(0.900000000041206,1.19310633605572,0.699999999958324));
#13372=CARTESIAN_POINT('Ctrl Pts',(0.900000000000325,1.18799600975363,0.7));
#13373=CARTESIAN_POINT('Ctrl Pts',(0.9,1.32024227787037,0.));
#13374=CARTESIAN_POINT('Ctrl Pts',(0.9,1.31486080448354,0.100670360916234));
#13375=CARTESIAN_POINT('Ctrl Pts',(0.9,1.30947907114291,0.201341392534));
#13376=CARTESIAN_POINT('Ctrl Pts',(0.9,1.2986918099064,0.403120086121531));
#13377=CARTESIAN_POINT('Ctrl Pts',(0.900000001878204,1.29328620583358,0.504229137772713));
#13378=CARTESIAN_POINT('Ctrl Pts',(0.900000001878204,1.28788040994396,0.605337476551879));
#13379=CARTESIAN_POINT('Ctrl Pts',(0.899999999999997,-1.32024227787137,
-1.86669707469278E-11));
#13380=CARTESIAN_POINT('Ctrl Pts',(0.909148787559422,-1.30966717532842,
0.201788252636133));
#13381=CARTESIAN_POINT('Ctrl Pts',(0.91829761066914,-1.29909207410335,0.403576503749508));
#13382=CARTESIAN_POINT('Ctrl Pts',(0.92744646984625,-1.28851697422138,0.605364753299354));
#13383=CARTESIAN_POINT('Ctrl Pts',(0.699273108318574,-1.31559634352334,
-5.7001548815619E-6));
#13384=CARTESIAN_POINT('Ctrl Pts',(0.708743431409066,-1.30502123870946,
0.20178254329682));
#13385=CARTESIAN_POINT('Ctrl Pts',(0.718213789763005,-1.2944461351935,0.403570785162392));
#13386=CARTESIAN_POINT('Ctrl Pts',(0.727684183892774,-1.28387103300525,
0.605359025419352));
#13387=CARTESIAN_POINT('Ctrl Pts',(0.498558799217305,-1.31100715552056,
-1.1774619888836E-5));
#13388=CARTESIAN_POINT('Ctrl Pts',(0.508350677965937,-1.30043204942944,
0.201776459055217));
#13389=CARTESIAN_POINT('Ctrl Pts',(0.518142591787393,-1.28985694462582,
0.403564691096996));
#13390=CARTESIAN_POINT('Ctrl Pts',(0.527934541191295,-1.27928184113929,
0.60535292148228));
#13391=CARTESIAN_POINT('Ctrl Pts',(0.29785707328833,-1.3064367443434,-1.84041486642056E-5));
#13392=CARTESIAN_POINT('Ctrl Pts',(0.307970527825607,-1.29586163794,0.20176981888596));
#13393=CARTESIAN_POINT('Ctrl Pts',(0.318084017341356,-1.28528653282298,
0.403558040236175));
#13394=CARTESIAN_POINT('Ctrl Pts',(0.328197542344371,-1.27471142901691,
0.605346259877786));
#13395=CARTESIAN_POINT('',(0.32957180616905,-1.2747428754212,0.605346305703265));
#13396=CARTESIAN_POINT('Ctrl Pts',(0.297857995688647,-1.306435779838,1.57426155444895E-16));
#13397=CARTESIAN_POINT('Ctrl Pts',(0.308429283449307,-1.29587142805659,
0.201782098465301));
#13398=CARTESIAN_POINT('Ctrl Pts',(0.319000553694994,-1.28530712634462,
0.403564200350135));
#13399=CARTESIAN_POINT('Ctrl Pts',(0.329571806169048,-1.2747428754212,0.605346305703266));
#13400=CARTESIAN_POINT('Ctrl Pts',(0.32957180616905,-1.2747428754212,0.605346305703265));
#13401=CARTESIAN_POINT('Ctrl Pts',(0.519721397561595,-1.27909449722757,
0.60534313598158));
#13402=CARTESIAN_POINT('Ctrl Pts',(0.709864288600121,-1.28346276435313,
0.605340219076093));
#13403=CARTESIAN_POINT('Ctrl Pts',(0.900000001879218,-1.28788040990034,
0.605337476551906));
#13404=CARTESIAN_POINT('Ctrl Pts',(0.90231940407953,-1.18804989493878,0.7));
#13405=CARTESIAN_POINT('Ctrl Pts',(0.712166351817731,-1.18363199317816,
0.7));
#13406=CARTESIAN_POINT('Ctrl Pts',(0.522011847238247,-1.17926361631973,
0.7));
#13407=CARTESIAN_POINT('Ctrl Pts',(0.331856371369203,-1.17491202960101,
0.7));
#13408=CARTESIAN_POINT('Ctrl Pts',(0.901648075315333,-1.21694488185794,
0.7));
#13409=CARTESIAN_POINT('Ctrl Pts',(0.711500071980331,-1.21252656425213,
0.69999998041973));
#13410=CARTESIAN_POINT('Ctrl Pts',(0.521348914609444,-1.20815772874132,
0.700000022626678));
#13411=CARTESIAN_POINT('Ctrl Pts',(0.331195161244126,-1.20380556524924,
0.7));
#13412=CARTESIAN_POINT('Ctrl Pts',(0.900484091294294,-1.26704448261357,
0.676664431332699));
#13413=CARTESIAN_POINT('Ctrl Pts',(0.710344780071471,-1.26262550764723,
0.676665329845182));
#13414=CARTESIAN_POINT('Ctrl Pts',(0.520199507967113,-1.25825584722226,
0.676666267597974));
#13415=CARTESIAN_POINT('Ctrl Pts',(0.3300487189482,-1.25390275839508,0.676667306001616));
#13416=CARTESIAN_POINT('Ctrl Pts',(0.90002687589075,-1.28672371253673,0.626983665342106));
#13417=CARTESIAN_POINT('Ctrl Pts',(0.709890987426059,-1.28230548388611,
0.626985988983916));
#13418=CARTESIAN_POINT('Ctrl Pts',(0.519747959090447,-1.27793661492756,
0.626988445273931));
#13419=CARTESIAN_POINT('Ctrl Pts',(0.329598318905021,-1.27358432286302,
0.626991130804315));
#13420=CARTESIAN_POINT('Ctrl Pts',(0.900000001879218,-1.28788040990034,
0.605337476551906));
#13421=CARTESIAN_POINT('Ctrl Pts',(0.709864288600121,-1.28346276435313,
0.605340219076093));
#13422=CARTESIAN_POINT('Ctrl Pts',(0.519721397561595,-1.27909449722757,
0.60534313598158));
#13423=CARTESIAN_POINT('Ctrl Pts',(0.32957180616905,-1.2747428754212,0.605346305703265));
#13424=CARTESIAN_POINT('',(0.331856371369201,-1.17491202962433,0.7));
#13425=CARTESIAN_POINT('Origin',(0.331856371539144,-1.1749120296049,0.6));
#13426=CARTESIAN_POINT('Ctrl Pts',(0.900000000000328,-1.18799600975363,
0.7));
#13427=CARTESIAN_POINT('Ctrl Pts',(0.71062007065371,-1.18359647108512,0.7));
#13428=CARTESIAN_POINT('Ctrl Pts',(0.521238702715143,-1.17924592340069,
0.7));
#13429=CARTESIAN_POINT('Ctrl Pts',(0.331856371369203,-1.17491202960101,
0.7));
#13430=CARTESIAN_POINT('Origin',(6.87409734069396,-2.22251806091942E-16,
0.7));
#13431=CARTESIAN_POINT('',(0.331856371879032,1.17491202961268,0.7));
#13432=CARTESIAN_POINT('',(0.331856371369201,-0.75,0.7));
#13433=CARTESIAN_POINT('Ctrl Pts',(0.331856371879031,1.17491202961268,0.7));
#13434=CARTESIAN_POINT('Ctrl Pts',(0.521238703055026,1.1792459234085,0.7));
#13435=CARTESIAN_POINT('Ctrl Pts',(0.710620070823648,1.18359647108907,0.7));
#13436=CARTESIAN_POINT('Ctrl Pts',(0.900000000000325,1.18799600975363,0.7));
#13437=CARTESIAN_POINT('Ctrl Pts',(0.297857073289265,1.30643674434242,-1.84041299971672E-5));
#13438=CARTESIAN_POINT('Ctrl Pts',(0.30797052782623,1.29586163793935,0.201769818898405));
#13439=CARTESIAN_POINT('Ctrl Pts',(0.318084017341667,1.28528653282265,0.403558040242397));
#13440=CARTESIAN_POINT('Ctrl Pts',(0.328197542344371,1.27471142901691,0.605346259877786));
#13441=CARTESIAN_POINT('Ctrl Pts',(0.49855879921793,1.31100715551957,-1.17746012218085E-5));
#13442=CARTESIAN_POINT('Ctrl Pts',(0.50835067796626,1.30043204942878,0.201776459067662));
#13443=CARTESIAN_POINT('Ctrl Pts',(0.518142591787414,1.28985694462549,0.403564691103219));
#13444=CARTESIAN_POINT('Ctrl Pts',(0.527934541191015,1.27928184113928,0.60535292148228));
#13445=CARTESIAN_POINT('Ctrl Pts',(0.699273108318888,1.31559634352235,-5.70013621459206E-6));
#13446=CARTESIAN_POINT('Ctrl Pts',(0.708743431409089,1.3050212387088,0.201782543309265));
#13447=CARTESIAN_POINT('Ctrl Pts',(0.718213789762737,1.29444613519316,0.403570785168614));
#13448=CARTESIAN_POINT('Ctrl Pts',(0.727684183892215,1.28387103300524,0.605359025419352));
#13449=CARTESIAN_POINT('Ctrl Pts',(0.9,1.32024227787037,-6.93889390390723E-18));
#13450=CARTESIAN_POINT('Ctrl Pts',(0.909148787559144,1.30966717532775,0.201788252648578));
#13451=CARTESIAN_POINT('Ctrl Pts',(0.918297610668582,1.29909207410301,0.403576503755731));
#13452=CARTESIAN_POINT('Ctrl Pts',(0.927446469845411,1.28851697422136,0.605364753299355));
#13453=CARTESIAN_POINT('',(0.329571806169048,1.2747428754212,0.605346305703265));
#13454=CARTESIAN_POINT('Ctrl Pts',(0.900000001879216,1.28788040990034,0.605337476551906));
#13455=CARTESIAN_POINT('Ctrl Pts',(0.709864288600119,1.28346276435313,0.605340219076093));
#13456=CARTESIAN_POINT('Ctrl Pts',(0.519721397561593,1.27909449722757,0.60534313598158));
#13457=CARTESIAN_POINT('Ctrl Pts',(0.329571806169048,1.2747428754212,0.605346305703265));
#13458=CARTESIAN_POINT('Ctrl Pts',(0.329571806169048,1.2747428754212,0.605346305703265));
#13459=CARTESIAN_POINT('Ctrl Pts',(0.319000553694994,1.28530712634462,0.403564200350134));
#13460=CARTESIAN_POINT('Ctrl Pts',(0.308429283449307,1.29587142805659,0.201782098465301));
#13461=CARTESIAN_POINT('Ctrl Pts',(0.297857995688647,1.306435779838,6.03900610074426E-17));
#13462=CARTESIAN_POINT('Ctrl Pts',(0.331856371369201,1.17491202960101,0.7));
#13463=CARTESIAN_POINT('Ctrl Pts',(0.522011847238246,1.17926361631973,0.7));
#13464=CARTESIAN_POINT('Ctrl Pts',(0.712166351817729,1.18363199317816,0.7));
#13465=CARTESIAN_POINT('Ctrl Pts',(0.902319404079528,1.18804989493878,0.7));
#13466=CARTESIAN_POINT('Ctrl Pts',(0.331195161244124,1.20380556524924,0.7));
#13467=CARTESIAN_POINT('Ctrl Pts',(0.521348914609443,1.20815772874132,0.700000022626678));
#13468=CARTESIAN_POINT('Ctrl Pts',(0.711500071980329,1.21252656425213,0.69999998041973));
#13469=CARTESIAN_POINT('Ctrl Pts',(0.901648075315331,1.21694488185794,0.7));
#13470=CARTESIAN_POINT('Ctrl Pts',(0.330048718948197,1.25390275839508,0.676667306001616));
#13471=CARTESIAN_POINT('Ctrl Pts',(0.52019950796711,1.25825584722226,0.676666267597973));
#13472=CARTESIAN_POINT('Ctrl Pts',(0.710344780071469,1.26262550764723,0.676665329845182));
#13473=CARTESIAN_POINT('Ctrl Pts',(0.900484091294292,1.26704448261357,0.676664431332698));
#13474=CARTESIAN_POINT('Ctrl Pts',(0.329598318905018,1.27358432286302,0.626991130804315));
#13475=CARTESIAN_POINT('Ctrl Pts',(0.519747959090446,1.27793661492756,0.62698844527393));
#13476=CARTESIAN_POINT('Ctrl Pts',(0.709890987426057,1.28230548388611,0.626985988983916));
#13477=CARTESIAN_POINT('Ctrl Pts',(0.900026875890748,1.28672371253673,0.626983665342106));
#13478=CARTESIAN_POINT('Ctrl Pts',(0.329571806169048,1.2747428754212,0.605346305703265));
#13479=CARTESIAN_POINT('Ctrl Pts',(0.519721397561593,1.27909449722757,0.60534313598158));
#13480=CARTESIAN_POINT('Ctrl Pts',(0.709864288600119,1.28346276435313,0.605340219076093));
#13481=CARTESIAN_POINT('Ctrl Pts',(0.900000001879216,1.28788040990034,0.605337476551906));
#13482=CARTESIAN_POINT('Origin',(0.331856371369202,1.17491202960101,0.6));
#13483=CARTESIAN_POINT('Origin',(0.331856371369202,1.17491202960101,0.6));
#13484=CARTESIAN_POINT('Origin',(0.331856371369201,1.17491202960879,0.6));
#13485=CARTESIAN_POINT('Origin',(0.331856371369202,1.17491202960101,0.6));
#13486=CARTESIAN_POINT('Origin',(12.8681436286308,1.83274446434879,0.6));
#13487=CARTESIAN_POINT('Origin',(12.8681436286308,1.83274446434879,0.6));
#13488=CARTESIAN_POINT('',(12.9680065821063,1.83274446434879,0.605233595624294));
#13489=CARTESIAN_POINT('Origin',(12.8681436286308,1.83274446434879,0.6));
#13490=CARTESIAN_POINT('Origin',(12.8681436286308,1.83274446434879,0.6));
#13491=CARTESIAN_POINT('Origin',(0.331856371369201,-1.17491202960101,0.6));
#13492=CARTESIAN_POINT('Origin',(0.331856371369201,-1.17491202960101,0.6));
#13493=CARTESIAN_POINT('Origin',(0.331856371369201,-1.17491202960101,0.6));
#13494=CARTESIAN_POINT('Origin',(0.331856371369201,-0.75,0.6));
#13495=CARTESIAN_POINT('Ctrl Pts',(0.297750759617602,-1.30654294555098,
-0.00204689530870639));
#13496=CARTESIAN_POINT('Ctrl Pts',(0.308357792853923,-1.29594287152607,
0.200417501569666));
#13497=CARTESIAN_POINT('Ctrl Pts',(0.318964808457496,-1.28534284790734,
0.40288190189057));
#13498=CARTESIAN_POINT('Ctrl Pts',(0.329571806169048,-1.2747428754212,0.605346305703266));
#13499=CARTESIAN_POINT('Ctrl Pts',(0.268364475985512,-1.30579334864515,
-0.000546070465277405));
#13500=CARTESIAN_POINT('Ctrl Pts',(0.278972236061358,-1.29519218153762,
0.201918231169276));
#13501=CARTESIAN_POINT('Ctrl Pts',(0.289579970322816,-1.28459115545203,
0.404382541571378));
#13502=CARTESIAN_POINT('Ctrl Pts',(0.300187702091134,-1.27399007937578,
0.606846849214128));
#13503=CARTESIAN_POINT('Ctrl Pts',(0.217994620733579,-1.28028753054242,
0.000758348866131992));
#13504=CARTESIAN_POINT('Ctrl Pts',(0.228604439653725,-1.26968580576698,
0.203222517770204));
#13505=CARTESIAN_POINT('Ctrl Pts',(0.239214264875756,-1.259084092946,0.405686686833815));
#13506=CARTESIAN_POINT('Ctrl Pts',(0.24982407554016,-1.24848245399652,0.608150860486448));
#13507=CARTESIAN_POINT('Ctrl Pts',(0.200221638751335,-1.22875730734246,
-0.00100806500432267));
#13508=CARTESIAN_POINT('Ctrl Pts',(0.210832346469089,-1.21815680658782,
0.201456130081263));
#13509=CARTESIAN_POINT('Ctrl Pts',(0.221443027663539,-1.20755634130466,
0.403920328365886));
#13510=CARTESIAN_POINT('Ctrl Pts',(0.232053735729819,-1.1969559383274,0.606384528499152));
#13511=CARTESIAN_POINT('Ctrl Pts',(0.200161316008396,-1.20671181983024,
-0.00215909150772397));
#13512=CARTESIAN_POINT('Ctrl Pts',(0.21077201649647,-1.19611183845239,0.200305134857769));
#13513=CARTESIAN_POINT('Ctrl Pts',(0.221382717124246,-1.18551190812967,
0.402769363888924));
#13514=CARTESIAN_POINT('Ctrl Pts',(0.231993417893744,-1.17491202960101,
0.605233595624295));
#13515=CARTESIAN_POINT('Origin',(12.8681436286308,-1.83274446434879,0.6));
#13516=CARTESIAN_POINT('',(12.9680065821063,-1.83274446434879,0.605233595624295));
#13517=CARTESIAN_POINT('Origin',(12.8681436286308,-1.83274446434879,0.6));
#13518=CARTESIAN_POINT('Origin',(12.8681436286308,-1.83274446434879,0.6));
#13519=CARTESIAN_POINT('Origin',(12.8681436286308,1.1,0.6));
#13520=CARTESIAN_POINT('',(12.9680065821063,1.1,0.605233595624295));
#13521=CARTESIAN_POINT('Ctrl Pts',(12.9998428721614,-1.86475648739599,-0.00223900654757928));
#13522=CARTESIAN_POINT('Ctrl Pts',(12.9892307746816,-1.85408610159386,0.200251876006837));
#13523=CARTESIAN_POINT('Ctrl Pts',(12.9786186779927,-1.84341542867022,0.402742743472647));
#13524=CARTESIAN_POINT('Ctrl Pts',(12.9680065821063,-1.83274446434879,0.605233595624296));
#13525=CARTESIAN_POINT('Ctrl Pts',(12.9997989521977,-1.88070362541494,-0.00140096371806573));
#13526=CARTESIAN_POINT('Ctrl Pts',(12.9891868560404,-1.87003481788623,0.2010900171988));
#13527=CARTESIAN_POINT('Ctrl Pts',(12.9785747412344,-1.85936572080465,0.403580981971657));
#13528=CARTESIAN_POINT('Ctrl Pts',(12.967962646681,-1.84869634914788,0.606071933479074));
#13529=CARTESIAN_POINT('Ctrl Pts',(12.9919061104719,-1.91252097257855,-0.00013797468654593));
#13530=CARTESIAN_POINT('Ctrl Pts',(12.9812924311808,-1.9018552985481,0.202353118580234));
#13531=CARTESIAN_POINT('Ctrl Pts',(12.970678744243,-1.89118929884075,0.404844194499128));
#13532=CARTESIAN_POINT('Ctrl Pts',(12.9600650516023,-1.88052308923615,0.607335259545336));
#13533=CARTESIAN_POINT('Ctrl Pts',(12.9539932318948,-1.95585643963679,0.000158685530800887));
#13534=CARTESIAN_POINT('Ctrl Pts',(12.9433725220626,-1.94519261899951,0.202649549046396));
#13535=CARTESIAN_POINT('Ctrl Pts',(12.9327517623504,-1.93452853669393,0.40514039680648));
#13536=CARTESIAN_POINT('Ctrl Pts',(12.9221309734579,-1.92386419524738,0.607631230057729));
#13537=CARTESIAN_POINT('Ctrl Pts',(12.9129235702791,-1.96658826742031,-0.00142816374191492));
#13538=CARTESIAN_POINT('Ctrl Pts',(12.9022969271978,-1.95592037993921,0.201062184830579));
#13539=CARTESIAN_POINT('Ctrl Pts',(12.891670251582,-1.94525202616943,0.403552507423554));
#13540=CARTESIAN_POINT('Ctrl Pts',(12.8810434760214,-1.93458357684419,0.60604282089977));
#13541=CARTESIAN_POINT('Ctrl Pts',(12.8891437477602,-1.96405813112492,-0.00280773857265357));
#13542=CARTESIAN_POINT('Ctrl Pts',(12.8785151960038,-1.95338599020215,0.199682283294402));
#13543=CARTESIAN_POINT('Ctrl Pts',(12.8678865709412,-1.94271355010484,0.402172286243574));
#13544=CARTESIAN_POINT('Ctrl Pts',(12.8572578715866,-1.93204080633595,0.604662269998931));
#13545=CARTESIAN_POINT('Ctrl Pts',(12.9997255308004,-1.86463850151065,-4.9439619065339E-17));
#13546=CARTESIAN_POINT('Ctrl Pts',(12.9891525471135,-1.85400744222428,0.201744546927532));
#13547=CARTESIAN_POINT('Ctrl Pts',(12.9785795642115,-1.84337609791338,0.403489078876654));
#13548=CARTESIAN_POINT('Ctrl Pts',(12.9680065821063,-1.83274446434879,0.605233595624296));
#13549=CARTESIAN_POINT('Ctrl Pts',(12.8891409639924,1.96405533594058,-0.00275470357795049));
#13550=CARTESIAN_POINT('Ctrl Pts',(12.8785133401458,1.95338412669368,0.199717639954231));
#13551=CARTESIAN_POINT('Ctrl Pts',(12.8678856430057,1.9427126183241,0.402189964571813));
#13552=CARTESIAN_POINT('Ctrl Pts',(12.8572578715866,1.93204080633595,0.604662269998929));
#13553=CARTESIAN_POINT('Ctrl Pts',(12.9049941793403,1.96574209420267,-0.00183498696757459));
#13554=CARTESIAN_POINT('Ctrl Pts',(12.8943678341644,1.95507368670196,0.20063757283533));
#13555=CARTESIAN_POINT('Ctrl Pts',(12.8837414238008,1.94440496992476,0.403110113573296));
#13556=CARTESIAN_POINT('Ctrl Pts',(12.8731149412098,1.93373598667478,0.605582637266155));
#13557=CARTESIAN_POINT('Ctrl Pts',(12.9374710816243,1.9613461313261,-0.000364592700753267));
#13558=CARTESIAN_POINT('Ctrl Pts',(12.9268487371951,1.95068187676899,0.202108391447626));
#13559=CARTESIAN_POINT('Ctrl Pts',(12.9162262930262,1.94001732715406,0.404581355450702));
#13560=CARTESIAN_POINT('Ctrl Pts',(12.9056038462248,1.92935253789361,0.607054307450502));
#13561=CARTESIAN_POINT('Ctrl Pts',(12.9846523118271,1.92834870343354,0.000369250346899581));
#13562=CARTESIAN_POINT('Ctrl Pts',(12.974038022963,1.91768545846127,0.202842678583437));
#13563=CARTESIAN_POINT('Ctrl Pts',(12.9634237233674,1.90702194269714,0.405316092420461));
#13564=CARTESIAN_POINT('Ctrl Pts',(12.9528094065597,1.89635817580376,0.607789492622546));
#13565=CARTESIAN_POINT('Ctrl Pts',(12.9997742127558,1.88867440031858,-0.000928907044737527));
#13566=CARTESIAN_POINT('Ctrl Pts',(12.9891630904765,1.8780073281596,0.201544447891303));
#13567=CARTESIAN_POINT('Ctrl Pts',(12.9785517991681,1.86733992038445,0.404017776344753));
#13568=CARTESIAN_POINT('Ctrl Pts',(12.9679406789684,1.85667229154743,0.606491102406462));
#13569=CARTESIAN_POINT('Ctrl Pts',(12.9998400927033,1.86475369267134,-0.00218597132744988));
#13570=CARTESIAN_POINT('Ctrl Pts',(12.9892289217097,1.85408423839396,0.200287232817622));
#13571=CARTESIAN_POINT('Ctrl Pts',(12.9786177515068,1.84341449704483,0.402760421876702));
#13572=CARTESIAN_POINT('Ctrl Pts',(12.9680065821063,1.83274446434879,0.605233595624294));
#13573=CARTESIAN_POINT('Ctrl Pts',(12.9680065821063,1.83274446434879,0.605233595624294));
#13574=CARTESIAN_POINT('Ctrl Pts',(12.9785795642115,1.84337609791338,0.403489078876654));
#13575=CARTESIAN_POINT('Ctrl Pts',(12.9891525471135,1.85400744222428,0.201744546927532));
#13576=CARTESIAN_POINT('Ctrl Pts',(12.9997255308004,1.86463850151065,1.86916454536501E-16));
#13577=CARTESIAN_POINT('Ctrl Pts',(12.6,1.80383022254432,0.7));
#13578=CARTESIAN_POINT('Ctrl Pts',(12.6893984576578,1.8133105623702,0.7));
#13579=CARTESIAN_POINT('Ctrl Pts',(12.7787800350189,1.82294762441299,0.7));
#13580=CARTESIAN_POINT('Ctrl Pts',(12.8681436286308,1.83274446434879,0.7));
#13581=CARTESIAN_POINT('Ctrl Pts',(12.5969393303222,1.83269196733649,0.7));
#13582=CARTESIAN_POINT('Ctrl Pts',(12.686303642571,1.84217134991284,0.700000098415946));
#13583=CARTESIAN_POINT('Ctrl Pts',(12.7756511334299,1.85180730951691,0.699999896874207));
#13584=CARTESIAN_POINT('Ctrl Pts',(12.8649798835675,1.86160311979107,0.7));
#13585=CARTESIAN_POINT('Ctrl Pts',(12.5916356538948,1.88270499442536,0.67643906321291));
#13586=CARTESIAN_POINT('Ctrl Pts',(12.6809412203008,1.89218243450198,0.676434576658958));
#13587=CARTESIAN_POINT('Ctrl Pts',(12.7702288461642,1.90181652272411,0.676430055978541));
#13588=CARTESIAN_POINT('Ctrl Pts',(12.8594976525144,1.91161025179704,0.676425356750174));
#13589=CARTESIAN_POINT('Ctrl Pts',(12.58957419749,1.90214427893475,0.626447702441804));
#13590=CARTESIAN_POINT('Ctrl Pts',(12.6788572782758,1.91161594713488,0.626436135819418));
#13591=CARTESIAN_POINT('Ctrl Pts',(12.7681225846323,1.92124403769089,0.626424372515079));
#13592=CARTESIAN_POINT('Ctrl Pts',(12.8573684983393,1.93103170500986,0.626412260100396));
#13593=CARTESIAN_POINT('Ctrl Pts',(12.5894662143615,1.90316254677271,0.604704117718382));
#13594=CARTESIAN_POINT('Ctrl Pts',(12.6787484942245,1.91263121188366,0.60469048808123));
#13595=CARTESIAN_POINT('Ctrl Pts',(12.7680127446979,1.92225628370762,0.604676541242762));
#13596=CARTESIAN_POINT('Ctrl Pts',(12.8572578715866,1.93204080633595,0.60466226999893));
#13597=CARTESIAN_POINT('Ctrl Pts',(0.200160815981423,1.20671231935208,-0.00216863259073552));
#13598=CARTESIAN_POINT('Ctrl Pts',(0.21077168314515,1.19611217146534,0.200298774135678));
#13599=CARTESIAN_POINT('Ctrl Pts',(0.221382550448584,1.18551207463533,0.402766183527835));
#13600=CARTESIAN_POINT('Ctrl Pts',(0.231993417893744,1.17491202960101,0.605233595624295));
#13601=CARTESIAN_POINT('Ctrl Pts',(0.200241246305444,1.23610630273461,-0.000633930584249493));
#13602=CARTESIAN_POINT('Ctrl Pts',(0.210852138766318,1.22550544237485,0.201833432539687));
#13603=CARTESIAN_POINT('Ctrl Pts',(0.221462948692539,1.21490467236247,0.404300804744641));
#13604=CARTESIAN_POINT('Ctrl Pts',(0.232073841675177,1.20430390790287,0.60676817279077));
#13605=CARTESIAN_POINT('Ctrl Pts',(0.224595236946023,1.28704077752974,0.000756396927320467));
#13606=CARTESIAN_POINT('Ctrl Pts',(0.235204871724134,1.27643877611169,0.203223757667495));
#13607=CARTESIAN_POINT('Ctrl Pts',(0.245814524913363,1.26583679641595,0.405691118453359));
#13608=CARTESIAN_POINT('Ctrl Pts',(0.256424148042823,1.25523487973404,0.608158484046399));
#13609=CARTESIAN_POINT('Ctrl Pts',(0.275710547013829,1.30598124743532,-0.000930817763883136));
#13610=CARTESIAN_POINT('Ctrl Pts',(0.286318282165364,1.29538020346814,0.201536689442792));
#13611=CARTESIAN_POINT('Ctrl Pts',(0.296926023167072,1.2847792285374,0.404004199876323));
#13612=CARTESIAN_POINT('Ctrl Pts',(0.307533728110612,1.27417827838713,0.606471713336412));
#13613=CARTESIAN_POINT('Ctrl Pts',(0.297750259763447,1.30654344507719,-0.0020564363997533));
#13614=CARTESIAN_POINT('Ctrl Pts',(0.308357459618374,1.29594320454196,0.200411140842193));
#13615=CARTESIAN_POINT('Ctrl Pts',(0.318964641840002,1.28534301441448,0.402878721526778));
#13616=CARTESIAN_POINT('Ctrl Pts',(0.329571806169048,1.2747428754212,0.605346305703265));
#13617=CARTESIAN_POINT('Origin',(13.0002740930491,2.2,-0.0104671912485888));
#13618=CARTESIAN_POINT('Origin',(0.331856371369202,1.17491202960101,0.6));
#13619=CARTESIAN_POINT('',(0.331856371879032,1.17491202961268,0.9));
#13620=CARTESIAN_POINT('',(0.0322675109428289,1.17491202960101,0.615700786872883));
#13621=CARTESIAN_POINT('Origin',(0.331856371369201,1.17491202962433,0.6));
#13622=CARTESIAN_POINT('',(0.325002675768741,1.47440456706157,0.616038917109795));
#13623=CARTESIAN_POINT('Origin',(0.331856371369202,1.17491202960101,0.6));
#13624=CARTESIAN_POINT('Origin',(0.331856371369201,1.17491202960101,0.6));
#13625=CARTESIAN_POINT('Origin',(12.8681436286308,1.83274446434879,0.6));
#13626=CARTESIAN_POINT('',(12.8681436286308,1.83274446434879,0.9));
#13627=CARTESIAN_POINT('',(12.8354863574981,2.13063349031027,0.613986809996789));
#13628=CARTESIAN_POINT('Origin',(12.8681436286308,1.83274446434879,0.6));
#13629=CARTESIAN_POINT('',(13.1677324890572,1.83274446434879,0.615700786872883));
#13630=CARTESIAN_POINT('Origin',(12.8681436286308,1.83274446434879,0.6));
#13631=CARTESIAN_POINT('Origin',(12.8681436286308,1.83274446434879,0.6));
#13632=CARTESIAN_POINT('Origin',(0.331856371369201,-1.17491202960101,0.6));
#13633=CARTESIAN_POINT('',(0.331856371369201,-1.17491202962433,0.9));
#13634=CARTESIAN_POINT('',(0.325002675768743,-1.47440456706157,0.616038917109795));
#13635=CARTESIAN_POINT('Origin',(0.331856371879032,-1.17491202961268,0.6));
#13636=CARTESIAN_POINT('',(0.0322675109428289,-1.17491202960101,0.615700786872884));
#13637=CARTESIAN_POINT('Origin',(0.331856371369201,-1.17491202960101,0.6));
#13638=CARTESIAN_POINT('Origin',(0.331856371369201,-1.17491202960101,0.6));
#13639=CARTESIAN_POINT('Origin',(0.331856371369201,-0.75,0.6));
#13640=CARTESIAN_POINT('',(0.0322675109428289,-0.75,0.615700786872883));
#13641=CARTESIAN_POINT('',(0.331856371369201,-0.75,0.9));
#13642=CARTESIAN_POINT('Ctrl Pts',(0.292429673212981,-1.5069793045954,-0.00614074949474724));
#13643=CARTESIAN_POINT('Ctrl Pts',(0.303287396789886,-1.49612100698918,
0.201252467440773));
#13644=CARTESIAN_POINT('Ctrl Pts',(0.314145064588525,-1.48526276089333,
0.408645689616972));
#13645=CARTESIAN_POINT('Ctrl Pts',(0.325002675768741,-1.47440456706157,
0.616038917109795));
#13646=CARTESIAN_POINT('Ctrl Pts',(0.204270663953122,-1.50473074636003,
-0.00163825452108868));
#13647=CARTESIAN_POINT('Ctrl Pts',(0.215130619942527,-1.49386909866124,
0.205754670272474));
#13648=CARTESIAN_POINT('Ctrl Pts',(0.225990497234893,-1.48300775583971,
0.413147615201549));
#13649=CARTESIAN_POINT('Ctrl Pts',(0.236850363534999,-1.47214617892531,
0.620540547642382));
#13650=CARTESIAN_POINT('Ctrl Pts',(0.0531014592841718,-1.42831231122466,
0.00228331220810075));
#13651=CARTESIAN_POINT('Ctrl Pts',(0.0639677431943945,-1.41744892560022,
0.209675827753147));
#13652=CARTESIAN_POINT('Ctrl Pts',(0.0748340498672138,-1.40658548887187,
0.417068339030394));
#13653=CARTESIAN_POINT('Ctrl Pts',(0.0857003072238147,-1.3957221574093,
0.624460858243749));
#13654=CARTESIAN_POINT('Ctrl Pts',(-0.000158492362241063,-1.27362248439808,
-0.0030242144278773));
#13655=CARTESIAN_POINT('Ctrl Pts',(0.0107105192099893,-1.2627628846508,
0.204368383073371));
#13656=CARTESIAN_POINT('Ctrl Pts',(0.0215794523842628,-1.25190326350425,
0.411760983371354));
#13657=CARTESIAN_POINT('Ctrl Pts',(0.0324484644510542,-1.24104375578019,
0.619153585497454));
#13658=CARTESIAN_POINT('Ctrl Pts',(-0.000339460947516079,-1.20748590713937,
-0.00647730073969574));
#13659=CARTESIAN_POINT('Ctrl Pts',(0.0105295295353408,-1.19662789414299,
0.200915392321314));
#13660=CARTESIAN_POINT('Ctrl Pts',(0.0213985201647323,-1.18576993469886,
0.408308088178364));
#13661=CARTESIAN_POINT('Ctrl Pts',(0.032267510942829,-1.17491202960101,
0.615700786872884));
#13662=CARTESIAN_POINT('Ctrl Pts',(0.292751161823634,-1.50665779898694,
4.33680868994202E-17));
#13663=CARTESIAN_POINT('Ctrl Pts',(0.30350172143464,-1.49590667092872,0.205346300540216));
#13664=CARTESIAN_POINT('Ctrl Pts',(0.314252226354851,-1.48515559337638,
0.410692606218909));
#13665=CARTESIAN_POINT('Ctrl Pts',(0.325002675768741,-1.47440456706157,
0.616038917109795));
#13666=CARTESIAN_POINT('Ctrl Pts',(0.032267510942829,-1.17491202960101,
0.615700786872884));
#13667=CARTESIAN_POINT('Ctrl Pts',(0.021511673816962,-1.18565689645617,
0.410467188483275));
#13668=CARTESIAN_POINT('Ctrl Pts',(0.0107558368367201,-1.19640181653194,
0.205233592872363));
#13669=CARTESIAN_POINT('Ctrl Pts',(-2.19605150036939E-16,-1.20714678905882,
1.11889664200504E-16));
#13670=CARTESIAN_POINT('Origin',(12.8681436286308,-1.83274446434879,0.6));
#13671=CARTESIAN_POINT('',(13.1677324890572,-1.83274446434879,0.615700786872883));
#13672=CARTESIAN_POINT('',(12.8354863574981,-2.13063349031027,0.613986809996789));
#13673=CARTESIAN_POINT('Origin',(12.8681436286308,-1.83274446434879,0.6));
#13674=CARTESIAN_POINT('',(12.8681436286308,-1.83274446434879,0.9));
#13675=CARTESIAN_POINT('Origin',(12.8681436286308,-1.83274446434879,0.6));
#13676=CARTESIAN_POINT('Origin',(12.8681436286308,-1.83274446434879,0.6));
#13677=CARTESIAN_POINT('Origin',(12.8681436286308,1.1,0.6));
#13678=CARTESIAN_POINT('',(13.1677324890572,1.1,0.615700786872883));
#13679=CARTESIAN_POINT('',(12.8681436286308,1.1,0.9));
#13680=CARTESIAN_POINT('Ctrl Pts',(12.8681436286308,-1.83274446434879,0.9));
#13681=CARTESIAN_POINT('Ctrl Pts',(11.0848390724976,-1.63724259846481,0.9));
#13682=CARTESIAN_POINT('Ctrl Pts',(6.90843812479705,-1.33014681916253,0.9));
#13683=CARTESIAN_POINT('Ctrl Pts',(2.72316671642812,-1.22963564084767,0.9));
#13684=CARTESIAN_POINT('Ctrl Pts',(0.331856371369203,-1.17491202960101,
0.9));
#13685=CARTESIAN_POINT('Ctrl Pts',(12.8586523934408,-1.91932043067563,0.9));
#13686=CARTESIAN_POINT('Ctrl Pts',(11.0774332085042,-1.7238803779394,0.89999435405169));
#13687=CARTESIAN_POINT('Ctrl Pts',(6.90489492800773,-1.41683381760594,0.900002805573959));
#13688=CARTESIAN_POINT('Ctrl Pts',(2.72111811994416,-1.31633797570969,0.90000078069347));
#13689=CARTESIAN_POINT('Ctrl Pts',(0.329872740993971,-1.26159263654569,
0.9));
#13690=CARTESIAN_POINT('Ctrl Pts',(12.8422006781022,-2.06938763738452,0.829321796184829));
#13691=CARTESIAN_POINT('Ctrl Pts',(11.0645720435655,-1.87407163985848,0.829602081442736));
#13692=CARTESIAN_POINT('Ctrl Pts',(6.89876476423634,-1.56711486110062,0.829953500700133));
#13693=CARTESIAN_POINT('Ctrl Pts',(2.71756729604702,-1.46664725828863,0.829952661937692));
#13694=CARTESIAN_POINT('Ctrl Pts',(0.326433810179884,-1.41186690836963,
0.829991693349937));
#13695=CARTESIAN_POINT('Ctrl Pts',(12.8358182377562,-2.12760618633201,0.679236780301187));
#13696=CARTESIAN_POINT('Ctrl Pts',(11.0595580661442,-1.93265366192027,0.679962478070753));
#13697=CARTESIAN_POINT('Ctrl Pts',(6.89634818471837,-1.62613750062048,0.680874066334139));
#13698=CARTESIAN_POINT('Ctrl Pts',(2.71617242066404,-1.52567909229178,0.680871998075852));
#13699=CARTESIAN_POINT('Ctrl Pts',(0.325082213976654,-1.47092890938704,
0.680973392412944));
#13700=CARTESIAN_POINT('Ctrl Pts',(12.8354863574981,-2.13063349031027,0.613986809996789));
#13701=CARTESIAN_POINT('Ctrl Pts',(11.0592740266891,-1.93586902238569,0.614841183901826));
#13702=CARTESIAN_POINT('Ctrl Pts',(6.89620783868867,-1.62958780289117,0.615922665333222));
#13703=CARTESIAN_POINT('Ctrl Pts',(2.71609101918193,-1.52912950204849,0.615919334096661));
#13704=CARTESIAN_POINT('Ctrl Pts',(0.325002675768742,-1.47440456706157,
0.616038917109795));
#13705=CARTESIAN_POINT('Ctrl Pts',(0.325002675768742,-1.47440456706157,
0.616038917109795));
#13706=CARTESIAN_POINT('Ctrl Pts',(2.71609101918193,-1.52912950204849,0.615919334096661));
#13707=CARTESIAN_POINT('Ctrl Pts',(6.89620783868867,-1.62958780289117,0.615922665333222));
#13708=CARTESIAN_POINT('Ctrl Pts',(11.0592740266891,-1.93586902238569,0.614841183901826));
#13709=CARTESIAN_POINT('Ctrl Pts',(12.8354863574981,-2.13063349031027,0.613986809996789));
#13710=CARTESIAN_POINT('Ctrl Pts',(12.8681436286308,-1.83274446434879,0.9));
#13711=CARTESIAN_POINT('Ctrl Pts',(11.0848390724976,-1.63724259846481,0.9));
#13712=CARTESIAN_POINT('Ctrl Pts',(6.90843812479705,-1.33014681916253,0.9));
#13713=CARTESIAN_POINT('Ctrl Pts',(2.72316671642812,-1.22963564084767,0.9));
#13714=CARTESIAN_POINT('Ctrl Pts',(0.331856371369203,-1.17491202960101,
0.9));
#13715=CARTESIAN_POINT('Ctrl Pts',(13.2003520234216,-1.86554403325358,-0.00671700702553119));
#13716=CARTESIAN_POINT('Ctrl Pts',(13.1894788444661,-1.85461114646479,0.200755606855839));
#13717=CARTESIAN_POINT('Ctrl Pts',(13.1786056663403,-1.84367795836273,0.40822820490283));
#13718=CARTESIAN_POINT('Ctrl Pts',(13.1677324890572,-1.83274446434879,0.615700786872884));
#13719=CARTESIAN_POINT('Ctrl Pts',(13.200220264666,-1.91338509859121,-0.00420290020003313));
#13720=CARTESIAN_POINT('Ctrl Pts',(13.1893470894366,-1.90245705934317,0.203270015787334));
#13721=CARTESIAN_POINT('Ctrl Pts',(13.1784738563058,-1.89152871992859,0.410742913234898));
#13722=CARTESIAN_POINT('Ctrl Pts',(13.1676006827814,-1.88060011874606,0.61821580043722));
#13723=CARTESIAN_POINT('Ctrl Pts',(13.1765676699515,-2.00888806967359,-0.000409897060868941));
#13724=CARTESIAN_POINT('Ctrl Pts',(13.1656896254949,-1.99796966505382,0.207063364242462));
#13725=CARTESIAN_POINT('Ctrl Pts',(13.1548115799789,-1.98705090404177,0.414536607525659));
#13726=CARTESIAN_POINT('Ctrl Pts',(13.1439334900924,-1.97613202744891,0.622009843787749));
#13727=CARTESIAN_POINT('Ctrl Pts',(13.0627995670833,-2.13884429305335,0.000475886042502645));
#13728=CARTESIAN_POINT('Ctrl Pts',(13.0518999280859,-2.12793157960824,0.207948441605934));
#13729=CARTESIAN_POINT('Ctrl Pts',(13.041000104914,-2.11701865581933,0.415420978499924));
#13730=CARTESIAN_POINT('Ctrl Pts',(13.0301002136907,-2.10610551685206,0.62289350259018));
#13731=CARTESIAN_POINT('Ctrl Pts',(12.9395973356642,-2.17103883395928,-0.00428435975826336));
#13732=CARTESIAN_POINT('Ctrl Pts',(12.9286794517625,-2.16011362679945,0.203186612960554));
#13733=CARTESIAN_POINT('Ctrl Pts',(12.9177614752639,-2.14918756369419,0.410657536673191));
#13734=CARTESIAN_POINT('Ctrl Pts',(12.9068431708026,-2.13826180183499,0.618128462699307));
#13735=CARTESIAN_POINT('Ctrl Pts',(12.8682582931239,-2.16344935299393,-0.00842301254802964));
#13736=CARTESIAN_POINT('Ctrl Pts',(12.857334548107,-2.15251107312608,0.1990469563258));
#13737=CARTESIAN_POINT('Ctrl Pts',(12.8464105706338,-2.1415724540018,0.406516897309109));
#13738=CARTESIAN_POINT('Ctrl Pts',(12.8354863574981,-2.13063349031027,0.61398680999679));
#13739=CARTESIAN_POINT('Ctrl Pts',(13.2,-1.86519007666192,-2.60208521396521E-17));
#13740=CARTESIAN_POINT('Ctrl Pts',(13.1892441622028,-1.85437516893481,0.20523361119958));
#13741=CARTESIAN_POINT('Ctrl Pts',(13.1784883252177,-1.84355996631422,0.410467206902138));
#13742=CARTESIAN_POINT('Ctrl Pts',(13.1677324890572,-1.83274446434879,0.615700786872884));
#13743=CARTESIAN_POINT('Ctrl Pts',(12.8354863574981,-2.13063349031027,0.61398680999679));
#13744=CARTESIAN_POINT('Ctrl Pts',(12.8462627343229,-2.14142441807303,0.409324567403199));
#13745=CARTESIAN_POINT('Ctrl Pts',(12.8570388818204,-2.15221501053143,0.204662297274642));
#13746=CARTESIAN_POINT('Ctrl Pts',(12.8678148030684,-2.16300527278357,2.15973072759112E-16));
#13747=CARTESIAN_POINT('Ctrl Pts',(12.868249917342,2.16344096606744,-0.0082639349430893));
#13748=CARTESIAN_POINT('Ctrl Pts',(12.8573289641336,2.15250548166836,0.19915300804817));
#13749=CARTESIAN_POINT('Ctrl Pts',(12.8464077785869,2.14156965818488,0.406569923163064));
#13750=CARTESIAN_POINT('Ctrl Pts',(12.8354863574981,2.13063349031027,0.613986809996789));
#13751=CARTESIAN_POINT('Ctrl Pts',(12.9158092820513,2.16850062662823,-0.00550483257449158));
#13752=CARTESIAN_POINT('Ctrl Pts',(12.9048922561706,2.15757374897544,0.201912774743134));
#13753=CARTESIAN_POINT('Ctrl Pts',(12.8939750281693,2.14664650750606,0.409330354360154));
#13754=CARTESIAN_POINT('Ctrl Pts',(12.8830575663678,2.13571903132675,0.616747911798467));
#13755=CARTESIAN_POINT('Ctrl Pts',(13.0132876381743,2.15534286385676,-0.00108956416640176));
#13756=CARTESIAN_POINT('Ctrl Pts',(13.002382910411,2.14442874534411,0.206329347217122));
#13757=CARTESIAN_POINT('Ctrl Pts',(12.9914779109393,2.13351435475356,0.413748232116966));
#13758=CARTESIAN_POINT('Ctrl Pts',(12.9805728576194,2.12259976690609,0.621167106093357));
#13759=CARTESIAN_POINT('Ctrl Pts',(13.1547834649542,2.05631410774027,0.001107541479323));
#13760=CARTESIAN_POINT('Ctrl Pts',(13.1439034803964,2.04540309863889,0.208527817346591));
#13761=CARTESIAN_POINT('Ctrl Pts',(13.1330234810862,2.03449182132921,0.415948079627069));
#13762=CARTESIAN_POINT('Ctrl Pts',(13.1221434051731,2.0235803832085,0.623368331037722));
#13763=CARTESIAN_POINT('Ctrl Pts',(13.2001460482598,1.93729725403583,-0.00278676680844524));
#13764=CARTESIAN_POINT('Ctrl Pts',(13.1892758011844,1.92637447722781,0.204633283810596));
#13765=CARTESIAN_POINT('Ctrl Pts',(13.1784050234814,1.91545126126866,0.412053283701094));
#13766=CARTESIAN_POINT('Ctrl Pts',(13.1675347796435,1.9045279459447,0.619473307219386));
#13767=CARTESIAN_POINT('Ctrl Pts',(13.2003436864113,1.86553565046225,-0.00655792739252892));
#13768=CARTESIAN_POINT('Ctrl Pts',(13.1894732864596,1.85460555778322,0.200861659936414));
#13769=CARTESIAN_POINT('Ctrl Pts',(13.1786028873373,1.84367516394377,0.408281231439009));
#13770=CARTESIAN_POINT('Ctrl Pts',(13.1677324890572,1.83274446434879,0.615700786872883));
#13771=CARTESIAN_POINT('Ctrl Pts',(12.8678148030684,2.16300527278357,-3.77302356024956E-17));
#13772=CARTESIAN_POINT('Ctrl Pts',(12.8570388818204,2.15221501053142,0.204662297274639));
#13773=CARTESIAN_POINT('Ctrl Pts',(12.8462627343229,2.14142441807303,0.409324567403198));
#13774=CARTESIAN_POINT('Ctrl Pts',(12.8354863574981,2.13063349031027,0.613986809996789));
#13775=CARTESIAN_POINT('Ctrl Pts',(13.1677324890572,1.83274446434879,0.615700786872883));
#13776=CARTESIAN_POINT('Ctrl Pts',(13.1784883252177,1.84355996631422,0.410467206902138));
#13777=CARTESIAN_POINT('Ctrl Pts',(13.1892441622028,1.85437516893481,0.20523361119958));
#13778=CARTESIAN_POINT('Ctrl Pts',(13.2,1.86519007666192,9.4542429440736E-17));
#13779=CARTESIAN_POINT('Ctrl Pts',(0.3318563713692,1.17491202960101,0.9));
#13780=CARTESIAN_POINT('Ctrl Pts',(2.72316671642811,1.22963564084767,0.9));
#13781=CARTESIAN_POINT('Ctrl Pts',(6.90843812479704,1.33014681916253,0.9));
#13782=CARTESIAN_POINT('Ctrl Pts',(11.0848390724976,1.63724259846481,0.9));
#13783=CARTESIAN_POINT('Ctrl Pts',(12.8681436286308,1.83274446434879,0.9));
#13784=CARTESIAN_POINT('Ctrl Pts',(0.329872740993969,1.26159263654569,0.9));
#13785=CARTESIAN_POINT('Ctrl Pts',(2.72111811994415,1.31633797570969,0.90000078069347));
#13786=CARTESIAN_POINT('Ctrl Pts',(6.90489492800774,1.41683381760594,0.90000280557396));
#13787=CARTESIAN_POINT('Ctrl Pts',(11.0774332085042,1.7238803779394,0.89999435405169));
#13788=CARTESIAN_POINT('Ctrl Pts',(12.8586523934408,1.91932043067563,0.9));
#13789=CARTESIAN_POINT('Ctrl Pts',(0.326433810179882,1.41186690836963,0.829991693349937));
#13790=CARTESIAN_POINT('Ctrl Pts',(2.71756729604703,1.46664725828863,0.829952661937692));
#13791=CARTESIAN_POINT('Ctrl Pts',(6.89876476423633,1.56711486110062,0.829953500700133));
#13792=CARTESIAN_POINT('Ctrl Pts',(11.0645720435655,1.87407163985848,0.829602081442736));
#13793=CARTESIAN_POINT('Ctrl Pts',(12.8422006781022,2.06938763738452,0.829321796184828));
#13794=CARTESIAN_POINT('Ctrl Pts',(0.325082213976652,1.47092890938703,0.680973392412944));
#13795=CARTESIAN_POINT('Ctrl Pts',(2.71617242066403,1.52567909229178,0.680871998075852));
#13796=CARTESIAN_POINT('Ctrl Pts',(6.89634818471838,1.62613750062048,0.680874066334139));
#13797=CARTESIAN_POINT('Ctrl Pts',(11.0595580661442,1.93265366192027,0.679962478070753));
#13798=CARTESIAN_POINT('Ctrl Pts',(12.8358182377562,2.12760618633201,0.679236780301187));
#13799=CARTESIAN_POINT('Ctrl Pts',(0.32500267576874,1.47440456706157,0.616038917109795));
#13800=CARTESIAN_POINT('Ctrl Pts',(2.71609101918192,1.52912950204849,0.615919334096661));
#13801=CARTESIAN_POINT('Ctrl Pts',(6.89620783868868,1.62958780289117,0.615922665333222));
#13802=CARTESIAN_POINT('Ctrl Pts',(11.0592740266891,1.93586902238569,0.614841183901826));
#13803=CARTESIAN_POINT('Ctrl Pts',(12.8354863574981,2.13063349031027,0.613986809996789));
#13804=CARTESIAN_POINT('Ctrl Pts',(12.8354863574981,2.13063349031027,0.613986809996789));
#13805=CARTESIAN_POINT('Ctrl Pts',(11.0592740266891,1.93586902238569,0.614841183901826));
#13806=CARTESIAN_POINT('Ctrl Pts',(6.89620783868868,1.62958780289117,0.615922665333222));
#13807=CARTESIAN_POINT('Ctrl Pts',(2.71609101918192,1.52912950204849,0.615919334096661));
#13808=CARTESIAN_POINT('Ctrl Pts',(0.32500267576874,1.47440456706157,0.616038917109795));
#13809=CARTESIAN_POINT('Ctrl Pts',(0.331856371879031,1.17491202961268,0.900000000000001));
#13810=CARTESIAN_POINT('Ctrl Pts',(2.72316671676804,1.22963564085583,0.9));
#13811=CARTESIAN_POINT('Ctrl Pts',(6.90843812496665,1.330146819175,0.9));
#13812=CARTESIAN_POINT('Ctrl Pts',(11.0848390724976,1.63724259846481,0.9));
#13813=CARTESIAN_POINT('Ctrl Pts',(12.8681436286308,1.83274446434879,0.9));
#13814=CARTESIAN_POINT('Ctrl Pts',(-0.00034095850043725,1.20748740317979,
-0.0065058757516861));
#13815=CARTESIAN_POINT('Ctrl Pts',(0.0105285311667133,1.19662889149835,
0.200896342313063));
#13816=CARTESIAN_POINT('Ctrl Pts',(0.0213980209804115,1.18577043337405,
0.408298563174108));
#13817=CARTESIAN_POINT('Ctrl Pts',(0.0322675109428289,1.17491202960101,
0.615700786872884));
#13818=CARTESIAN_POINT('Ctrl Pts',(-9.96670524854573E-5,1.295669506487,
-0.00190176065173685));
#13819=CARTESIAN_POINT('Ctrl Pts',(0.0107698931059531,1.28480880908357,
0.205500324005663));
#13820=CARTESIAN_POINT('Ctrl Pts',(0.0216392211477595,1.27394827585187,
0.412902429485043));
#13821=CARTESIAN_POINT('Ctrl Pts',(0.0325087822871292,1.26308766450658,
0.62030451837231));
#13822=CARTESIAN_POINT('Ctrl Pts',(0.0728623575603101,1.44853010213391,
0.00227745497540766));
#13823=CARTESIAN_POINT('Ctrl Pts',(0.0837280751164453,1.43766588856392,
0.209679530627308));
#13824=CARTESIAN_POINT('Ctrl Pts',(0.0945938325013454,1.42680163888532,
0.41708160190494));
#13825=CARTESIAN_POINT('Ctrl Pts',(0.105459512942901,1.41593747613444,0.624483681552028));
#13826=CARTESIAN_POINT('Ctrl Pts',(0.226308920038025,1.50529438233544,-0.00279245331904538));
#13827=CARTESIAN_POINT('Ctrl Pts',(0.237168779176494,1.4944331215396,0.204610074087555));
#13828=CARTESIAN_POINT('Ctrl Pts',(0.248028678199983,1.48357195724705,0.412012604182119));
#13829=CARTESIAN_POINT('Ctrl Pts',(0.258888441593434,1.47271077595937,0.619415140009235));
#13830=CARTESIAN_POINT('Ctrl Pts',(0.292428177212438,1.50698080067503,-0.00616932457891824));
#13831=CARTESIAN_POINT('Ctrl Pts',(0.303286399461314,1.49612200437087,0.201233417384176));
#13832=CARTESIAN_POINT('Ctrl Pts',(0.314144565926839,1.48526325958177,0.408636164588429));
#13833=CARTESIAN_POINT('Ctrl Pts',(0.325002675768741,1.47440456706157,0.616038917109795));
#13834=CARTESIAN_POINT('Ctrl Pts',(1.62630325872826E-19,1.20714678905882,
-9.93129189996722E-17));
#13835=CARTESIAN_POINT('Ctrl Pts',(0.0107558368367203,1.19640181653194,
0.205233592872363));
#13836=CARTESIAN_POINT('Ctrl Pts',(0.0215116738169619,1.18565689645617,
0.410467188483274));
#13837=CARTESIAN_POINT('Ctrl Pts',(0.0322675109428289,1.17491202960101,
0.615700786872884));
#13838=CARTESIAN_POINT('Ctrl Pts',(0.325002675768741,1.47440456706157,0.616038917109795));
#13839=CARTESIAN_POINT('Ctrl Pts',(0.314252226354851,1.48515559337638,0.410692606218907));
#13840=CARTESIAN_POINT('Ctrl Pts',(0.30350172143464,1.49590667092872,0.205346300540215));
#13841=CARTESIAN_POINT('Ctrl Pts',(0.292751161823635,1.50665779898694,-1.27502175484295E-16));
#13842=CARTESIAN_POINT('Ctrl Pts',(12.8678148030684,-2.16300527278356,0.));
#13843=CARTESIAN_POINT('Ctrl Pts',(12.8575947095063,-2.15224352891768,0.205346305703265));
#13844=CARTESIAN_POINT('Ctrl Pts',(12.8473746159443,-2.14148178505179,0.41069261140653));
#13845=CARTESIAN_POINT('Ctrl Pts',(12.8371545223823,-2.13072004118591,0.616038917109795));
#13846=CARTESIAN_POINT('Ctrl Pts',(8.67612692265345,-1.70561506876628,0.));
#13847=CARTESIAN_POINT('Ctrl Pts',(8.67274165808153,-1.69485332490039,0.205346305703265));
#13848=CARTESIAN_POINT('Ctrl Pts',(8.66935639350961,-1.68409158103451,0.41069261140653));
#13849=CARTESIAN_POINT('Ctrl Pts',(8.6659711289377,-1.67332983716862,0.616038917109795));
#13850=CARTESIAN_POINT('Ctrl Pts',(4.48443904223854,-1.60211086545473,0.));
#13851=CARTESIAN_POINT('Ctrl Pts',(4.48788860665674,-1.59134912158884,0.205346305703265));
#13852=CARTESIAN_POINT('Ctrl Pts',(4.49133817107494,-1.58058737772296,0.41069261140653));
#13853=CARTESIAN_POINT('Ctrl Pts',(4.49478773549313,-1.56982563385707,0.616038917109795));
#13854=CARTESIAN_POINT('Ctrl Pts',(0.292751161823634,-1.50665779898694,
0.));
#13855=CARTESIAN_POINT('Ctrl Pts',(0.303035555231945,-1.49589605512106,
0.205346305703265));
#13856=CARTESIAN_POINT('Ctrl Pts',(0.313319948640256,-1.48513431125517,
0.41069261140653));
#13857=CARTESIAN_POINT('Ctrl Pts',(0.323604342048567,-1.47437256738929,
0.616038917109795));
#13858=CARTESIAN_POINT('Origin',(0.,-1.5,0.));
#13859=CARTESIAN_POINT('Origin',(6.87409734069396,-2.22044604925031E-16,
0.9));
#13860=CARTESIAN_POINT('Ctrl Pts',(0.292751161823634,1.50665779898694,0.));
#13861=CARTESIAN_POINT('Ctrl Pts',(0.303035555231945,1.49589605512106,0.205346305703265));
#13862=CARTESIAN_POINT('Ctrl Pts',(0.313319948640256,1.48513431125517,0.41069261140653));
#13863=CARTESIAN_POINT('Ctrl Pts',(0.323604342048567,1.47437256738929,0.616038917109795));
#13864=CARTESIAN_POINT('Ctrl Pts',(4.48443904223854,1.60211086545473,0.));
#13865=CARTESIAN_POINT('Ctrl Pts',(4.48788860665674,1.59134912158884,0.205346305703265));
#13866=CARTESIAN_POINT('Ctrl Pts',(4.49133817107493,1.58058737772296,0.41069261140653));
#13867=CARTESIAN_POINT('Ctrl Pts',(4.49478773549313,1.56982563385707,0.616038917109795));
#13868=CARTESIAN_POINT('Ctrl Pts',(8.67612692265345,1.70561506876628,0.));
#13869=CARTESIAN_POINT('Ctrl Pts',(8.67274165808153,1.69485332490039,0.205346305703265));
#13870=CARTESIAN_POINT('Ctrl Pts',(8.66935639350961,1.68409158103451,0.41069261140653));
#13871=CARTESIAN_POINT('Ctrl Pts',(8.66597112893769,1.67332983716862,0.616038917109795));
#13872=CARTESIAN_POINT('Ctrl Pts',(12.8678148030684,2.16300527278356,0.));
#13873=CARTESIAN_POINT('Ctrl Pts',(12.8575947095063,2.15224352891768,0.205346305703265));
#13874=CARTESIAN_POINT('Ctrl Pts',(12.8473746159443,2.14148178505179,0.41069261140653));
#13875=CARTESIAN_POINT('Ctrl Pts',(12.8371545223823,2.13072004118591,0.616038917109795));
#13876=CARTESIAN_POINT('Origin',(13.2,2.2,0.));
#13877=CARTESIAN_POINT('',(0.,0.,0.));
#13878=CARTESIAN_POINT('Origin',(2.,0.,1.));
#13879=CARTESIAN_POINT('',(1.65,4.28626379701574E-17,1.1));
#13880=CARTESIAN_POINT('Origin',(2.,0.,1.1));
#13881=CARTESIAN_POINT('',(1.65,4.28626379701574E-17,0.9));
#13882=CARTESIAN_POINT('',(1.65,4.28626379701574E-17,1.));
#13883=CARTESIAN_POINT('Origin',(2.,0.,0.9));
#13884=CARTESIAN_POINT('Origin',(11.2,0.,1.));
#13885=CARTESIAN_POINT('',(10.85,4.28626379701574E-17,1.1));
#13886=CARTESIAN_POINT('Origin',(11.2,0.,1.1));
#13887=CARTESIAN_POINT('',(10.85,4.28626379701574E-17,0.9));
#13888=CARTESIAN_POINT('',(10.85,4.28626379701574E-17,1.));
#13889=CARTESIAN_POINT('Origin',(11.2,0.,0.9));
#13890=CARTESIAN_POINT('Origin',(9.9,1.,0.7));
#13891=CARTESIAN_POINT('',(9.65,1.,0.7));
#13892=CARTESIAN_POINT('Origin',(9.9,1.,0.7));
#13893=CARTESIAN_POINT('',(9.75,1.,0.7));
#13894=CARTESIAN_POINT('Origin',(9.9,1.,0.7));
#13895=CARTESIAN_POINT('Origin',(9.9,1.,0.7));
#13896=CARTESIAN_POINT('',(9.65,1.,0.6));
#13897=CARTESIAN_POINT('Origin',(9.9,1.,0.6));
#13898=CARTESIAN_POINT('',(9.65,1.,0.7));
#13899=CARTESIAN_POINT('Origin',(9.9,1.,0.6));
#13900=CARTESIAN_POINT('Origin',(3.3,-1.,0.7));
#13901=CARTESIAN_POINT('',(3.05,-1.,0.7));
#13902=CARTESIAN_POINT('Origin',(3.3,-1.,0.7));
#13903=CARTESIAN_POINT('',(3.15,-1.,0.7));
#13904=CARTESIAN_POINT('Origin',(3.3,-1.,0.7));
#13905=CARTESIAN_POINT('Origin',(3.3,-1.,0.7));
#13906=CARTESIAN_POINT('',(3.05,-1.,0.6));
#13907=CARTESIAN_POINT('Origin',(3.3,-1.,0.6));
#13908=CARTESIAN_POINT('',(3.05,-1.,0.7));
#13909=CARTESIAN_POINT('Origin',(3.3,-1.,0.6));
#13910=CARTESIAN_POINT('Origin',(3.3,1.,0.7));
#13911=CARTESIAN_POINT('',(3.05,1.,0.7));
#13912=CARTESIAN_POINT('Origin',(3.3,1.,0.7));
#13913=CARTESIAN_POINT('',(3.15,1.,0.7));
#13914=CARTESIAN_POINT('Origin',(3.3,1.,0.7));
#13915=CARTESIAN_POINT('Origin',(3.3,1.,0.7));
#13916=CARTESIAN_POINT('',(3.05,1.,0.6));
#13917=CARTESIAN_POINT('Origin',(3.3,1.,0.6));
#13918=CARTESIAN_POINT('',(3.05,1.,0.7));
#13919=CARTESIAN_POINT('Origin',(3.3,1.,0.6));
#13920=CARTESIAN_POINT('Origin',(9.9,-1.,0.7));
#13921=CARTESIAN_POINT('',(9.65,-1.,0.7));
#13922=CARTESIAN_POINT('Origin',(9.9,-1.,0.7));
#13923=CARTESIAN_POINT('',(9.75,-1.,0.7));
#13924=CARTESIAN_POINT('Origin',(9.9,-1.,0.7));
#13925=CARTESIAN_POINT('Origin',(9.9,-1.,0.7));
#13926=CARTESIAN_POINT('',(9.65,-1.,0.6));
#13927=CARTESIAN_POINT('Origin',(9.9,-1.,0.6));
#13928=CARTESIAN_POINT('',(9.65,-1.,0.7));
#13929=CARTESIAN_POINT('Origin',(9.9,-1.,0.6));
#13930=CARTESIAN_POINT('Origin',(9.9,1.,0.9));
#13931=CARTESIAN_POINT('',(9.75,1.,0.9));
#13932=CARTESIAN_POINT('',(9.75,1.,0.9));
#13933=CARTESIAN_POINT('Origin',(9.9,1.,0.9));
#13934=CARTESIAN_POINT('Origin',(3.3,-1.,0.9));
#13935=CARTESIAN_POINT('',(3.15,-1.,0.9));
#13936=CARTESIAN_POINT('',(3.15,-1.,0.9));
#13937=CARTESIAN_POINT('Origin',(3.3,-1.,0.9));
#13938=CARTESIAN_POINT('Origin',(3.3,1.,0.9));
#13939=CARTESIAN_POINT('',(3.15,1.,0.9));
#13940=CARTESIAN_POINT('',(3.15,1.,0.9));
#13941=CARTESIAN_POINT('Origin',(3.3,1.,0.9));
#13942=CARTESIAN_POINT('Origin',(9.9,-1.,0.9));
#13943=CARTESIAN_POINT('',(9.75,-1.,0.9));
#13944=CARTESIAN_POINT('',(9.75,-1.,0.9));
#13945=CARTESIAN_POINT('Origin',(9.9,-1.,0.9));
#13946=CARTESIAN_POINT('Ctrl Pts',(12.6883460378814,1.74710477827991,1.1));
#13947=CARTESIAN_POINT('Ctrl Pts',(12.7050904406715,1.74907248191433,1.1));
#13948=CARTESIAN_POINT('Ctrl Pts',(12.7459721545883,1.73893278412019,1.1));
#13949=CARTESIAN_POINT('Ctrl Pts',(12.7664342774515,1.70015954799943,1.1));
#13950=CARTESIAN_POINT('Ctrl Pts',(12.7664342774515,1.67768005087614,1.1));
#13951=CARTESIAN_POINT('Ctrl Pts',(12.6856343728622,1.77018000694724,1.1));
#13952=CARTESIAN_POINT('Ctrl Pts',(12.70797027111,1.77258660535003,1.09999193474305));
#13953=CARTESIAN_POINT('Ctrl Pts',(12.7620607807224,1.75878051965913,1.09998076816122));
#13954=CARTESIAN_POINT('Ctrl Pts',(12.789311301819,1.70760782583852,1.09999039212455));
#13955=CARTESIAN_POINT('Ctrl Pts',(12.7895723566779,1.67768005087614,1.1));
#13956=CARTESIAN_POINT('Ctrl Pts',(12.6809355967604,1.81016478834023,1.08112516654061));
#13957=CARTESIAN_POINT('Ctrl Pts',(12.7128933108791,1.81335099699619,1.08149246505882));
#13958=CARTESIAN_POINT('Ctrl Pts',(12.7898658458254,1.7931743676233,1.08208124913004));
#13959=CARTESIAN_POINT('Ctrl Pts',(12.8289908274994,1.72043204305838,1.08173005449524));
#13960=CARTESIAN_POINT('Ctrl Pts',(12.829672543413,1.67768005087614,1.08128963884528));
#13961=CARTESIAN_POINT('Ctrl Pts',(12.6791127113589,1.82567684354491,1.04109086533338));
#13962=CARTESIAN_POINT('Ctrl Pts',(12.7147851087716,1.82957775596959,1.04203732134162));
#13963=CARTESIAN_POINT('Ctrl Pts',(12.8014031907485,1.80754024306994,1.04357783697133));
#13964=CARTESIAN_POINT('Ctrl Pts',(12.8450621014111,1.72550665092358,1.04265503156396));
#13965=CARTESIAN_POINT('Ctrl Pts',(12.8454164251054,1.67768005087614,1.0415166534692));
#13966=CARTESIAN_POINT('Ctrl Pts',(12.6790190612712,1.82647376985122,1.02368384096639));
#13967=CARTESIAN_POINT('Ctrl Pts',(12.7148414907177,1.83063166001164,1.02479882190871));
#13968=CARTESIAN_POINT('Ctrl Pts',(12.8023492944496,1.80880756543048,1.02662811038865));
#13969=CARTESIAN_POINT('Ctrl Pts',(12.8462542441509,1.7257797841646,1.02553011374107));
#13970=CARTESIAN_POINT('Ctrl Pts',(12.8463246402318,1.67768005087614,1.02418687649944));
#13971=CARTESIAN_POINT('',(12.7664342774515,1.67768005087614,1.1));
#13972=CARTESIAN_POINT('',(12.8463246402318,1.67768005087614,1.02418687649944));
#13973=CARTESIAN_POINT('Origin',(12.7664342774515,1.67768005087614,1.02));
#13974=CARTESIAN_POINT('',(12.6790190612712,1.82647376985123,1.02368384096637));
#13975=CARTESIAN_POINT('Ctrl Pts',(12.8463246402318,1.67768005087614,1.02418687649944));
#13976=CARTESIAN_POINT('Ctrl Pts',(12.8462542441509,1.7257797841646,1.02553011374107));
#13977=CARTESIAN_POINT('Ctrl Pts',(12.8023492944496,1.80880756543048,1.02662811038865));
#13978=CARTESIAN_POINT('Ctrl Pts',(12.7148414907177,1.83063166001164,1.02479882190871));
#13979=CARTESIAN_POINT('Ctrl Pts',(12.6790190612712,1.82647376985122,1.02368384096639));
#13980=CARTESIAN_POINT('',(12.6883460378814,1.74710477827991,1.1));
#13981=CARTESIAN_POINT('Origin',(12.6883460378814,1.74710477827991,1.02));
#13982=CARTESIAN_POINT('Ctrl Pts',(12.6883460378814,1.74710477827991,1.1));
#13983=CARTESIAN_POINT('Ctrl Pts',(12.7050904406715,1.74907248191433,1.1));
#13984=CARTESIAN_POINT('Ctrl Pts',(12.7459721545883,1.73893278412019,1.1));
#13985=CARTESIAN_POINT('Ctrl Pts',(12.7664342774515,1.70015954799943,1.1));
#13986=CARTESIAN_POINT('Ctrl Pts',(12.7664342774515,1.67768005087614,1.1));
#13987=CARTESIAN_POINT('Origin',(12.7664342774515,0.926416499322631,1.02));
#13988=CARTESIAN_POINT('',(12.7664342774515,-1.67768005087614,1.1));
#13989=CARTESIAN_POINT('',(12.8463246402318,-1.67768005087614,1.02418687649944));
#13990=CARTESIAN_POINT('Origin',(12.7664342774515,-1.67768005087614,1.02));
#13991=CARTESIAN_POINT('',(12.8463246402318,0.926416499322631,1.02418687649944));
#13992=CARTESIAN_POINT('',(12.7664342774515,0.926416499322631,1.1));
#13993=CARTESIAN_POINT('Ctrl Pts',(12.7664342774515,-1.67768005087614,1.1));
#13994=CARTESIAN_POINT('Ctrl Pts',(12.7664342774515,-1.69453967371875,1.1));
#13995=CARTESIAN_POINT('Ctrl Pts',(12.7515713182712,-1.73395715258217,1.1));
#13996=CARTESIAN_POINT('Ctrl Pts',(12.7106719082684,-1.74972838312583,1.1));
#13997=CARTESIAN_POINT('Ctrl Pts',(12.6883460378814,-1.74710477827991,1.1));
#13998=CARTESIAN_POINT('Ctrl Pts',(12.7895723566779,-1.67768005087614,1.1));
#13999=CARTESIAN_POINT('Ctrl Pts',(12.7893765655337,-1.70012588209812,1.09999279409341));
#14000=CARTESIAN_POINT('Ctrl Pts',(12.7694119126837,-1.75223468493452,1.09998162170574));
#14001=CARTESIAN_POINT('Ctrl Pts',(12.7154155705261,-1.77338880481765,1.09998924632407));
#14002=CARTESIAN_POINT('Ctrl Pts',(12.6856343728622,-1.77018000694724,1.1));
#14003=CARTESIAN_POINT('Ctrl Pts',(12.829672543413,-1.67768005087614,1.08128963884528));
#14004=CARTESIAN_POINT('Ctrl Pts',(12.8291612564778,-1.70974404501309,1.08161995058275));
#14005=CARTESIAN_POINT('Ctrl Pts',(12.800330508486,-1.78383870138124,1.08209231231141));
#14006=CARTESIAN_POINT('Ctrl Pts',(12.7235458822523,-1.81441306654821,1.08161489789823));
#14007=CARTESIAN_POINT('Ctrl Pts',(12.6809355967604,-1.81016478834023,1.08112516654061));
#14008=CARTESIAN_POINT('Ctrl Pts',(12.8454164251054,-1.67768005087614,1.0415166534692));
#14009=CARTESIAN_POINT('Ctrl Pts',(12.8451506823347,-1.71355000091203,1.04237043704028));
#14010=CARTESIAN_POINT('Ctrl Pts',(12.8132193893781,-1.79702133948082,1.04360777159741));
#14011=CARTESIAN_POINT('Ctrl Pts',(12.7266759079096,-1.8308780601112,1.04235280667771));
#14012=CARTESIAN_POINT('Ctrl Pts',(12.6791127113589,-1.82567684354491,1.04109086533338));
#14013=CARTESIAN_POINT('Ctrl Pts',(12.8463246402318,-1.67768005087614,1.02418687649944));
#14014=CARTESIAN_POINT('Ctrl Pts',(12.8462718431712,-1.71375485084279,1.02519430443067));
#14015=CARTESIAN_POINT('Ctrl Pts',(12.8143456047297,-1.79814359426379,1.02666431898144));
#14016=CARTESIAN_POINT('Ctrl Pts',(12.7267823005336,-1.83201762339849,1.02517048222283));
#14017=CARTESIAN_POINT('Ctrl Pts',(12.6790190612712,-1.82647376985122,1.02368384096639));
#14018=CARTESIAN_POINT('',(12.6883460378814,-1.74710477827991,1.1));
#14019=CARTESIAN_POINT('',(12.6790190612712,-1.82647376985122,1.02368384096639));
#14020=CARTESIAN_POINT('Origin',(12.6883460378814,-1.74710477827991,1.02));
#14021=CARTESIAN_POINT('Ctrl Pts',(12.6790190612712,-1.82647376985122,1.02368384096639));
#14022=CARTESIAN_POINT('Ctrl Pts',(12.7267823005336,-1.83201762339849,1.02517048222283));
#14023=CARTESIAN_POINT('Ctrl Pts',(12.8143456047297,-1.79814359426379,1.02666431898144));
#14024=CARTESIAN_POINT('Ctrl Pts',(12.8462718431712,-1.71375485084279,1.02519430443067));
#14025=CARTESIAN_POINT('Ctrl Pts',(12.8463246402318,-1.67768005087614,1.02418687649944));
#14026=CARTESIAN_POINT('Ctrl Pts',(12.7664342774515,-1.67768005087614,1.1));
#14027=CARTESIAN_POINT('Ctrl Pts',(12.7664342774515,-1.69453967371875,1.1));
#14028=CARTESIAN_POINT('Ctrl Pts',(12.7515713182712,-1.73395715258217,1.1));
#14029=CARTESIAN_POINT('Ctrl Pts',(12.7106719082684,-1.74972838312583,1.1));
#14030=CARTESIAN_POINT('Ctrl Pts',(12.6883460378814,-1.74710477827991,1.1));
#14031=CARTESIAN_POINT('Ctrl Pts',(12.6883460378814,-1.74710477827991,1.1));
#14032=CARTESIAN_POINT('Ctrl Pts',(10.9559705848985,-1.54352621428166,1.1));
#14033=CARTESIAN_POINT('Ctrl Pts',(6.89625808461774,-1.22619725057464,1.1));
#14034=CARTESIAN_POINT('Ctrl Pts',(2.82684345252479,-1.12583341467021,1.1));
#14035=CARTESIAN_POINT('Ctrl Pts',(0.501786340825443,-1.06996858265586,
1.1));
#14036=CARTESIAN_POINT('Ctrl Pts',(12.6856343728622,-1.77018000694724,1.1));
#14037=CARTESIAN_POINT('Ctrl Pts',(10.953864459251,-1.56662322149928,1.09999817462394));
#14038=CARTESIAN_POINT('Ctrl Pts',(6.89527069668598,-1.24931220526659,1.1000008953949));
#14039=CARTESIAN_POINT('Ctrl Pts',(2.8262782431937,-1.14895306774358,1.10000025453557));
#14040=CARTESIAN_POINT('Ctrl Pts',(0.501230998995504,-1.09308153985212,
1.1));
#14041=CARTESIAN_POINT('Ctrl Pts',(12.6809355941985,-1.8101648101409,1.08112518582372));
#14042=CARTESIAN_POINT('Ctrl Pts',(10.9502073547204,-1.60665097561358,1.08120831496985));
#14043=CARTESIAN_POINT('Ctrl Pts',(6.89356335983392,-1.28937229578717,1.08131090328882));
#14044=CARTESIAN_POINT('Ctrl Pts',(2.82529878789426,-1.18902174359502,1.08130951558098));
#14045=CARTESIAN_POINT('Ctrl Pts',(0.500268515819014,-1.13313944880305,
1.0813211979534));
#14046=CARTESIAN_POINT('Ctrl Pts',(12.6791127113589,-1.82567684354491,1.04109086533338));
#14047=CARTESIAN_POINT('Ctrl Pts',(10.9487809439014,-1.62227255850559,1.04130507278566));
#14048=CARTESIAN_POINT('Ctrl Pts',(6.89288912441654,-1.30512519378816,1.04157208078929));
#14049=CARTESIAN_POINT('Ctrl Pts',(2.82491362604336,-1.2047760518259,1.04156824165415));
#14050=CARTESIAN_POINT('Ctrl Pts',(0.499889770467655,-1.14890257814483,
1.04159845594383));
#14051=CARTESIAN_POINT('Ctrl Pts',(12.6790190612712,-1.82647376985122,1.02368384096639));
#14052=CARTESIAN_POINT('Ctrl Pts',(10.9487001718726,-1.62312516854374,1.02393618996614));
#14053=CARTESIAN_POINT('Ctrl Pts',(6.89285005483575,-1.30604661809728,1.02425267661394));
#14054=CARTESIAN_POINT('Ctrl Pts',(2.82489114035621,-1.20569670918473,1.0242479474763));
#14055=CARTESIAN_POINT('Ctrl Pts',(0.499867468581681,-1.14983076778971,
1.024283610038));
#14056=CARTESIAN_POINT('',(0.501786340825443,-1.06996858265586,1.1));
#14057=CARTESIAN_POINT('',(0.499867468607324,-1.1498307677904,1.02428361003669));
#14058=CARTESIAN_POINT('Origin',(0.501786340825443,-1.06996858265586,1.02));
#14059=CARTESIAN_POINT('Ctrl Pts',(0.499867468581681,-1.14983076778971,
1.024283610038));
#14060=CARTESIAN_POINT('Ctrl Pts',(2.82489114035621,-1.20569670918473,1.0242479474763));
#14061=CARTESIAN_POINT('Ctrl Pts',(6.89285005483575,-1.30604661809728,1.02425267661394));
#14062=CARTESIAN_POINT('Ctrl Pts',(10.9487001718726,-1.62312516854374,1.02393618996614));
#14063=CARTESIAN_POINT('Ctrl Pts',(12.6790190612712,-1.82647376985122,1.02368384096639));
#14064=CARTESIAN_POINT('Ctrl Pts',(12.6883460378814,-1.74710477827991,1.1));
#14065=CARTESIAN_POINT('Ctrl Pts',(10.9559705848985,-1.54352621428166,1.1));
#14066=CARTESIAN_POINT('Ctrl Pts',(6.89625808461774,-1.22619725057464,1.1));
#14067=CARTESIAN_POINT('Ctrl Pts',(2.82684345252479,-1.12583341467021,1.1));
#14068=CARTESIAN_POINT('Ctrl Pts',(0.501786340825443,-1.06996858265586,
1.1));
#14069=CARTESIAN_POINT('Ctrl Pts',(0.501786340845132,-1.06996858265633,
1.1));
#14070=CARTESIAN_POINT('Ctrl Pts',(0.486343670353271,-1.06959753705714,
1.1));
#14071=CARTESIAN_POINT('Ctrl Pts',(0.450546621606563,-1.05636265633066,
1.1));
#14072=CARTESIAN_POINT('Ctrl Pts',(0.4335657225485,-1.02068090721437,1.1));
#14073=CARTESIAN_POINT('Ctrl Pts',(0.433565722548536,-1.00008473726807,
1.1));
#14074=CARTESIAN_POINT('Ctrl Pts',(0.501230999004731,-1.09308153985199,
1.1));
#14075=CARTESIAN_POINT('Ctrl Pts',(0.480678852604012,-1.0924131923446,1.09999359215549));
#14076=CARTESIAN_POINT('Ctrl Pts',(0.433334506735602,-1.0746197149398,1.09998454864803));
#14077=CARTESIAN_POINT('Ctrl Pts',(0.410665947227687,-1.02750530853182,
1.09999122945172));
#14078=CARTESIAN_POINT('Ctrl Pts',(0.410427643322096,-1.00008473726803,
1.1));
#14079=CARTESIAN_POINT('Ctrl Pts',(0.500268097562941,-1.13315685597024,
1.08133662520967));
#14080=CARTESIAN_POINT('Ctrl Pts',(0.470917694462572,-1.13199579109467,
1.08163072487897));
#14081=CARTESIAN_POINT('Ctrl Pts',(0.403559863183325,-1.10627672518437,
1.08206304806334));
#14082=CARTESIAN_POINT('Ctrl Pts',(0.370932263602498,-1.0392553542177,1.08170715357768));
#14083=CARTESIAN_POINT('Ctrl Pts',(0.370309959289207,-1.00008473726796,
1.08130512018932));
#14084=CARTESIAN_POINT('Ctrl Pts',(0.4998897704516,-1.14890257814396,1.04159845594539));
#14085=CARTESIAN_POINT('Ctrl Pts',(0.467042111092653,-1.1478756708603,1.04235909019736));
#14086=CARTESIAN_POINT('Ctrl Pts',(0.391210771603448,-1.11942230347982,
1.04349095641912));
#14087=CARTESIAN_POINT('Ctrl Pts',(0.354907019248534,-1.04390490695311,
1.04255582181557));
#14088=CARTESIAN_POINT('Ctrl Pts',(0.354583574894623,-1.00008473726793,
1.04151665346919));
#14089=CARTESIAN_POINT('Ctrl Pts',(0.499867468565196,-1.14983076778922,
1.02428361003984));
#14090=CARTESIAN_POINT('Ctrl Pts',(0.466823083113769,-1.14898864521809,
1.02518140264794));
#14091=CARTESIAN_POINT('Ctrl Pts',(0.390185579422885,-1.12055776822857,
1.0265258196442));
#14092=CARTESIAN_POINT('Ctrl Pts',(0.353739620824501,-1.04415516223227,
1.0254130505005));
#14093=CARTESIAN_POINT('Ctrl Pts',(0.353675359768169,-1.00008473726793,
1.02418687649943));
#14094=CARTESIAN_POINT('',(0.433565722548536,-1.00008473726807,1.1));
#14095=CARTESIAN_POINT('',(0.353675359768456,-1.00008473726778,1.0241868765049));
#14096=CARTESIAN_POINT('Origin',(0.433565722548536,-1.00008473726807,1.02));
#14097=CARTESIAN_POINT('Ctrl Pts',(0.353675359768169,-1.00008473726793,
1.02418687649943));
#14098=CARTESIAN_POINT('Ctrl Pts',(0.353739620824501,-1.04415516223227,
1.0254130505005));
#14099=CARTESIAN_POINT('Ctrl Pts',(0.390185579422885,-1.12055776822857,
1.0265258196442));
#14100=CARTESIAN_POINT('Ctrl Pts',(0.466823083113769,-1.14898864521809,
1.02518140264794));
#14101=CARTESIAN_POINT('Ctrl Pts',(0.499867468565196,-1.14983076778922,
1.02428361003984));
#14102=CARTESIAN_POINT('Ctrl Pts',(0.501786340845132,-1.06996858265633,
1.1));
#14103=CARTESIAN_POINT('Ctrl Pts',(0.486343670353271,-1.06959753705714,
1.1));
#14104=CARTESIAN_POINT('Ctrl Pts',(0.450546621606563,-1.05636265633066,
1.1));
#14105=CARTESIAN_POINT('Ctrl Pts',(0.4335657225485,-1.02068090721437,1.1));
#14106=CARTESIAN_POINT('Ctrl Pts',(0.433565722548536,-1.00008473726807,
1.1));
#14107=CARTESIAN_POINT('Origin',(0.433565722548535,-0.576416499322632,1.02));
#14108=CARTESIAN_POINT('',(0.433565722548535,1.0000847372682,1.1));
#14109=CARTESIAN_POINT('',(0.35367535976817,1.0000847372682,1.02418687649944));
#14110=CARTESIAN_POINT('Origin',(0.433565722548535,1.0000847372682,1.02));
#14111=CARTESIAN_POINT('',(0.35367535976817,-0.576416499322632,1.02418687649944));
#14112=CARTESIAN_POINT('',(0.433565722548535,-0.576416499322632,1.1));
#14113=CARTESIAN_POINT('Ctrl Pts',(0.433565722548535,1.0000847372682,1.1));
#14114=CARTESIAN_POINT('Ctrl Pts',(0.433565722548535,1.01553186472631,1.1));
#14115=CARTESIAN_POINT('Ctrl Pts',(0.445933851022605,1.05163704585376,1.1));
#14116=CARTESIAN_POINT('Ctrl Pts',(0.481196113556474,1.06947385520094,1.1));
#14117=CARTESIAN_POINT('Ctrl Pts',(0.501786340877041,1.0699685826571,1.1));
#14118=CARTESIAN_POINT('Ctrl Pts',(0.410427643322096,1.0000847372682,1.1));
#14119=CARTESIAN_POINT('Ctrl Pts',(0.410606371251307,1.0206501657139,1.09999342208879));
#14120=CARTESIAN_POINT('Ctrl Pts',(0.427269489276852,1.06840883688971,1.09998438534344));
#14121=CARTESIAN_POINT('Ctrl Pts',(0.473828137181897,1.09219040985597,1.09999145620732));
#14122=CARTESIAN_POINT('Ctrl Pts',(0.501230999047159,1.09308153985336,1.1));
#14123=CARTESIAN_POINT('Ctrl Pts',(0.370309959289211,1.0000847372682,1.08130512018932));
#14124=CARTESIAN_POINT('Ctrl Pts',(0.370776687524182,1.02946269997745,1.08160664523056));
#14125=CARTESIAN_POINT('Ctrl Pts',(0.394906927696186,1.09741901043509,1.08206104999852));
#14126=CARTESIAN_POINT('Ctrl Pts',(0.461134226826275,1.13160876948958,1.08172875810162));
#14127=CARTESIAN_POINT('Ctrl Pts',(0.500268097623607,1.13315685597264,1.08133662520906));
#14128=CARTESIAN_POINT('Ctrl Pts',(0.354583574894625,1.0000847372682,1.0415166534692));
#14129=CARTESIAN_POINT('Ctrl Pts',(0.354826158160091,1.03294986452867,1.0422960297289));
#14130=CARTESIAN_POINT('Ctrl Pts',(0.381463759848658,1.10944036955345,1.04348552759116));
#14131=CARTESIAN_POINT('Ctrl Pts',(0.456092891378057,1.14753336845448,1.04261263494683));
#14132=CARTESIAN_POINT('Ctrl Pts',(0.499889770519448,1.14890257814608,1.04159845594382));
#14133=CARTESIAN_POINT('Ctrl Pts',(0.35367535976817,1.0000847372682,1.02418687649944));
#14134=CARTESIAN_POINT('Ctrl Pts',(0.353723555560473,1.03313755598801,1.02510650700014));
#14135=CARTESIAN_POINT('Ctrl Pts',(0.380300727059747,1.11043180383933,1.02651925632578));
#14136=CARTESIAN_POINT('Ctrl Pts',(0.455808288035698,1.1487079377163,1.02548066684923));
#14137=CARTESIAN_POINT('Ctrl Pts',(0.499867468633476,1.14983076779096,1.02428361003799));
#14138=CARTESIAN_POINT('',(0.501786340877041,1.0699685826571,1.1));
#14139=CARTESIAN_POINT('',(0.499867468633699,1.14983076779054,1.0242836100458));
#14140=CARTESIAN_POINT('Origin',(0.501786340877041,1.0699685826571,1.02));
#14141=CARTESIAN_POINT('Ctrl Pts',(0.499867468633476,1.14983076779096,1.02428361003799));
#14142=CARTESIAN_POINT('Ctrl Pts',(0.455808288035698,1.1487079377163,1.02548066684923));
#14143=CARTESIAN_POINT('Ctrl Pts',(0.380300727059747,1.11043180383933,1.02651925632578));
#14144=CARTESIAN_POINT('Ctrl Pts',(0.353723555560473,1.03313755598801,1.02510650700014));
#14145=CARTESIAN_POINT('Ctrl Pts',(0.35367535976817,1.0000847372682,1.02418687649944));
#14146=CARTESIAN_POINT('Ctrl Pts',(0.433565722548535,1.0000847372682,1.1));
#14147=CARTESIAN_POINT('Ctrl Pts',(0.433565722548535,1.01553186472631,1.1));
#14148=CARTESIAN_POINT('Ctrl Pts',(0.445933851022605,1.05163704585376,1.1));
#14149=CARTESIAN_POINT('Ctrl Pts',(0.481196113556474,1.06947385520094,1.1));
#14150=CARTESIAN_POINT('Ctrl Pts',(0.501786340877041,1.0699685826571,1.1));
#14151=CARTESIAN_POINT('Ctrl Pts',(0.501786340877248,1.0699685826571,1.1));
#14152=CARTESIAN_POINT('Ctrl Pts',(2.82684356715236,1.12583341742443,1.1));
#14153=CARTESIAN_POINT('Ctrl Pts',(6.89625445951469,1.22619710828032,1.1));
#14154=CARTESIAN_POINT('Ctrl Pts',(10.9559704995293,1.54352620424957,1.1));
#14155=CARTESIAN_POINT('Ctrl Pts',(12.6883460378814,1.74710477827991,1.1));
#14156=CARTESIAN_POINT('Ctrl Pts',(0.501230999047308,1.09308153985337,1.1));
#14157=CARTESIAN_POINT('Ctrl Pts',(2.82627835782077,1.14895307049812,1.10000025453558));
#14158=CARTESIAN_POINT('Ctrl Pts',(6.89526707210341,1.24931206297629,1.10000089539479));
#14159=CARTESIAN_POINT('Ctrl Pts',(10.9538643739116,1.56662321146826,1.09999817462385));
#14160=CARTESIAN_POINT('Ctrl Pts',(12.6856343728622,1.77018000694724,1.1));
#14161=CARTESIAN_POINT('Ctrl Pts',(0.500268515870817,1.1331394488043,1.0813211979534));
#14162=CARTESIAN_POINT('Ctrl Pts',(2.82529890252049,1.18902174635009,1.08130951558041));
#14163=CARTESIAN_POINT('Ctrl Pts',(6.89355973615254,1.28937215350496,1.08131090331441));
#14164=CARTESIAN_POINT('Ctrl Pts',(10.9502072694324,1.60665096558469,1.08120831497395));
#14165=CARTESIAN_POINT('Ctrl Pts',(12.6809355941985,1.8101648101409,1.08112518582372));
#14166=CARTESIAN_POINT('Ctrl Pts',(0.499889770519458,1.14890257814608,1.04159845594383));
#14167=CARTESIAN_POINT('Ctrl Pts',(2.82491374066927,1.20477605458053,1.04156824165266));
#14168=CARTESIAN_POINT('Ctrl Pts',(6.89288550108907,1.30512505153819,1.04157208085565));
#14169=CARTESIAN_POINT('Ctrl Pts',(10.948780858633,1.62227254848209,1.04130507279621));
#14170=CARTESIAN_POINT('Ctrl Pts',(12.6791127113589,1.82567684354491,1.04109086533338));
#14171=CARTESIAN_POINT('Ctrl Pts',(0.499867468633484,1.14983076779096,1.024283610038));
#14172=CARTESIAN_POINT('Ctrl Pts',(2.82489125498211,1.205696711939,1.02424794747454));
#14173=CARTESIAN_POINT('Ctrl Pts',(6.89284643152835,1.3060464758645,1.02425267669241));
#14174=CARTESIAN_POINT('Ctrl Pts',(10.9487000866048,1.62312515852299,1.02393618997858));
#14175=CARTESIAN_POINT('Ctrl Pts',(12.6790190612712,1.82647376985123,1.02368384096639));
#14176=CARTESIAN_POINT('Ctrl Pts',(12.6790190612712,1.82647376985123,1.02368384096639));
#14177=CARTESIAN_POINT('Ctrl Pts',(10.9487000866048,1.62312515852299,1.02393618997858));
#14178=CARTESIAN_POINT('Ctrl Pts',(6.89284643152835,1.3060464758645,1.02425267669241));
#14179=CARTESIAN_POINT('Ctrl Pts',(2.82489125498211,1.205696711939,1.02424794747454));
#14180=CARTESIAN_POINT('Ctrl Pts',(0.499867468633484,1.14983076779096,1.024283610038));
#14181=CARTESIAN_POINT('Ctrl Pts',(0.501786340877248,1.0699685826571,1.1));
#14182=CARTESIAN_POINT('Ctrl Pts',(2.82684356715236,1.12583341742443,1.1));
#14183=CARTESIAN_POINT('Ctrl Pts',(6.89625445951469,1.22619710828032,1.1));
#14184=CARTESIAN_POINT('Ctrl Pts',(10.9559704995293,1.54352620424957,1.1));
#14185=CARTESIAN_POINT('Ctrl Pts',(12.6883460378814,1.74710477827991,1.1));
#14186=CARTESIAN_POINT('Origin',(0.347167001354737,-1.15283299864526,0.9));
#14187=CARTESIAN_POINT('',(0.347167001354737,1.00658943961019,0.9));
#14188=CARTESIAN_POINT('Ctrl Pts',(0.347167001354737,1.00658943961019,0.9));
#14189=CARTESIAN_POINT('Ctrl Pts',(0.349336454155793,1.00442120424608,0.941395625434512));
#14190=CARTESIAN_POINT('Ctrl Pts',(0.351505906960267,1.0022529701308,0.982791250934257));
#14191=CARTESIAN_POINT('Ctrl Pts',(0.35367535976817,1.0000847372682,1.02418687649944));
#14192=CARTESIAN_POINT('',(0.347167001354737,-1.00658943961019,0.9));
#14193=CARTESIAN_POINT('',(0.347167001354737,-1.15283299864526,0.9));
#14194=CARTESIAN_POINT('Ctrl Pts',(0.353675359768457,-1.00008473726791,
1.02418687650491));
#14195=CARTESIAN_POINT('Ctrl Pts',(0.351505906960458,-1.0022529701306,0.982791250937906));
#14196=CARTESIAN_POINT('Ctrl Pts',(0.349336454155888,-1.00442120424599,
0.941395625436337));
#14197=CARTESIAN_POINT('Ctrl Pts',(0.347167001354737,-1.00658943961019,
0.900000000000001));
#14198=CARTESIAN_POINT('Ctrl Pts',(0.346996296805428,1.00676004836741,0.896742763161407));
#14199=CARTESIAN_POINT('Ctrl Pts',(0.349222651122738,1.0045349433512,0.939224134205317));
#14200=CARTESIAN_POINT('Ctrl Pts',(0.351449005443648,1.00230983965007,0.981705505317921));
#14201=CARTESIAN_POINT('Ctrl Pts',(0.35367535976817,1.0000847372682,1.02418687649944));
#14202=CARTESIAN_POINT('Ctrl Pts',(0.347116900426942,1.05081591929015,0.899044017348554));
#14203=CARTESIAN_POINT('Ctrl Pts',(0.349343263597644,1.04859056550012,0.941525373982715));
#14204=CARTESIAN_POINT('Ctrl Pts',(0.351569598045448,1.04636522758029,0.98400673296308));
#14205=CARTESIAN_POINT('Ctrl Pts',(0.353795961241832,1.04413987589222,1.02648808970312));
#14206=CARTESIAN_POINT('Ctrl Pts',(0.383592239441417,1.12715274970112,0.901130824661994));
#14207=CARTESIAN_POINT('Ctrl Pts',(0.38581816402279,1.12492699736917,0.943612181832344));
#14208=CARTESIAN_POINT('Ctrl Pts',(0.388044096297176,1.12270123909217,0.986093538279035));
#14209=CARTESIAN_POINT('Ctrl Pts',(0.390270019973987,1.12047548800691,1.02857489555427));
#14210=CARTESIAN_POINT('Ctrl Pts',(0.460164343209507,1.15561854687756,0.898608842835867));
#14211=CARTESIAN_POINT('Ctrl Pts',(0.462389604568499,1.15339312775892,0.941090251624243));
#14212=CARTESIAN_POINT('Ctrl Pts',(0.464614871986574,1.15116771740584,0.983571660556392));
#14213=CARTESIAN_POINT('Ctrl Pts',(0.466840131020026,1.14894230022584,1.02605306955844));
#14214=CARTESIAN_POINT('Ctrl Pts',(0.493196683694039,1.15650174777388,0.896923951850831));
#14215=CARTESIAN_POINT('Ctrl Pts',(0.49542175781822,1.15427660869429,0.939405385103827));
#14216=CARTESIAN_POINT('Ctrl Pts',(0.497646830577711,1.15205147087705,0.981886818489558));
#14217=CARTESIAN_POINT('Ctrl Pts',(0.499871901968125,1.1498263343261,1.02436825200844));
#14218=CARTESIAN_POINT('',(0.493357799610229,1.15634062715414,0.9));
#14219=CARTESIAN_POINT('Ctrl Pts',(0.499867468633513,1.14983076779054,1.02428361004581));
#14220=CARTESIAN_POINT('Ctrl Pts',(0.497697580259738,1.1520007197087,0.982855739904038));
#14221=CARTESIAN_POINT('Ctrl Pts',(0.495527690583954,1.15417067283112,0.941427869888898));
#14222=CARTESIAN_POINT('Ctrl Pts',(0.493357799610229,1.15634062715414,0.9));
#14223=CARTESIAN_POINT('Ctrl Pts',(0.493357799610229,1.15634062715414,0.9));
#14224=CARTESIAN_POINT('Ctrl Pts',(0.482602647031033,1.1560824793541,0.899999999999731));
#14225=CARTESIAN_POINT('Ctrl Pts',(0.471926867235344,1.1546337250523,0.899998382330426));
#14226=CARTESIAN_POINT('Ctrl Pts',(0.461511103461674,1.15208577142905,0.899997935562642));
#14227=CARTESIAN_POINT('Ctrl Pts',(0.453002267216956,1.15000429947842,0.899997570589511));
#14228=CARTESIAN_POINT('Ctrl Pts',(0.444666263429443,1.14718801542572,0.899997957558805));
#14229=CARTESIAN_POINT('Ctrl Pts',(0.436607964282466,1.14366186386534,0.899998978246166));
#14230=CARTESIAN_POINT('Ctrl Pts',(0.426757323168539,1.13935141908028,0.900000225956719));
#14231=CARTESIAN_POINT('Ctrl Pts',(0.417425277328103,1.13402704260718,0.900002535631972));
#14232=CARTESIAN_POINT('Ctrl Pts',(0.408793513884033,1.1277570068973,0.900002417864976));
#14233=CARTESIAN_POINT('Ctrl Pts',(0.406442206080559,1.1260490379535,0.900002385785035));
#14234=CARTESIAN_POINT('Ctrl Pts',(0.404142986411405,1.12427063023042,0.900002152965402));
#14235=CARTESIAN_POINT('Ctrl Pts',(0.40189988757483,1.12242258952304,0.900001599918915));
#14236=CARTESIAN_POINT('Ctrl Pts',(0.397433290854798,1.11874265691041,0.900000498658648));
#14237=CARTESIAN_POINT('Ctrl Pts',(0.393188994678067,1.11478677136369,0.899998147353889));
#14238=CARTESIAN_POINT('Ctrl Pts',(0.389180227688998,1.11057998277971,0.899995556820878));
#14239=CARTESIAN_POINT('Ctrl Pts',(0.381747711834384,1.10278032195316,0.899990753803459));
#14240=CARTESIAN_POINT('Ctrl Pts',(0.375201641992584,1.09420365251288,0.899985427555825));
#14241=CARTESIAN_POINT('Ctrl Pts',(0.369602030462105,1.08503231460429,0.899982994308828));
#14242=CARTESIAN_POINT('Ctrl Pts',(0.365103987453251,1.07766518348509,0.899981039735804));
#14243=CARTESIAN_POINT('Ctrl Pts',(0.361217082581294,1.06991300661492,0.899980859474918));
#14244=CARTESIAN_POINT('Ctrl Pts',(0.357992910300892,1.06185737523451,0.899982473761482));
#14245=CARTESIAN_POINT('Ctrl Pts',(0.354005020049728,1.0518935857546,0.899984470428251));
#14246=CARTESIAN_POINT('Ctrl Pts',(0.351071168910505,1.04156966067519,0.899989252895565));
#14247=CARTESIAN_POINT('Ctrl Pts',(0.349267161175031,1.03104850244781,0.899993624760896));
#14248=CARTESIAN_POINT('Ctrl Pts',(0.347885225415831,1.022988911296,0.899996973769283));
#14249=CARTESIAN_POINT('Ctrl Pts',(0.347167001481006,1.014812725533,0.899999999989923));
#14250=CARTESIAN_POINT('Ctrl Pts',(0.347167001354737,1.00658943961019,0.900000000000001));
#14251=CARTESIAN_POINT('Ctrl Pts',(0.493357799610229,1.15634062715414,0.9));
#14252=CARTESIAN_POINT('Ctrl Pts',(0.495478181125715,1.15416948447463,0.941427870236244));
#14253=CARTESIAN_POINT('Ctrl Pts',(0.4975985626412,1.15199834179512,0.982855740472488));
#14254=CARTESIAN_POINT('Ctrl Pts',(0.499718944156686,1.14982719911562,1.02428361070873));
#14255=CARTESIAN_POINT('Ctrl Pts',(4.55741138981048,1.2538870134557,0.9));
#14256=CARTESIAN_POINT('Ctrl Pts',(4.55812062853622,1.25171587077619,0.941427870236244));
#14257=CARTESIAN_POINT('Ctrl Pts',(4.55882986726197,1.24954472809669,0.982855740472489));
#14258=CARTESIAN_POINT('Ctrl Pts',(4.55953910598771,1.24737358541718,1.02428361070873));
#14259=CARTESIAN_POINT('Ctrl Pts',(8.62146498001072,1.3558778793304,0.9));
#14260=CARTESIAN_POINT('Ctrl Pts',(8.62076307594673,1.35370673665089,0.941427870236244));
#14261=CARTESIAN_POINT('Ctrl Pts',(8.62006117188274,1.35153559397139,0.982855740472488));
#14262=CARTESIAN_POINT('Ctrl Pts',(8.61935926781874,1.34936445129188,1.02428361070873));
#14263=CARTESIAN_POINT('Ctrl Pts',(12.685518570211,1.83297820604925,0.9));
#14264=CARTESIAN_POINT('Ctrl Pts',(12.6834055233572,1.83080706336974,0.941427870236244));
#14265=CARTESIAN_POINT('Ctrl Pts',(12.6812924765035,1.82863592069023,0.982855740472488));
#14266=CARTESIAN_POINT('Ctrl Pts',(12.6791794296498,1.82646477801072,1.02428361070873));
#14267=CARTESIAN_POINT('',(12.685518570211,1.83297820604925,0.9));
#14268=CARTESIAN_POINT('Ctrl Pts',(12.685518570211,1.83297820604925,0.9));
#14269=CARTESIAN_POINT('Ctrl Pts',(12.6833520729681,1.83081006895277,0.941227947697879));
#14270=CARTESIAN_POINT('Ctrl Pts',(12.6811855699938,1.8286419235626,0.982455894687412));
#14271=CARTESIAN_POINT('Ctrl Pts',(12.6790190612712,1.82647376985122,1.02368384096639));
#14272=CARTESIAN_POINT('Ctrl Pts',(0.493357799610229,1.15634062715414,0.9));
#14273=CARTESIAN_POINT('Ctrl Pts',(4.55741138981048,1.2538870134557,0.9));
#14274=CARTESIAN_POINT('Ctrl Pts',(8.62146498001073,1.3558778793304,0.9));
#14275=CARTESIAN_POINT('Ctrl Pts',(12.685518570211,1.83297820604925,0.9));
#14276=CARTESIAN_POINT('Ctrl Pts',(12.6857396223418,1.83319942548878,0.895793428058847));
#14277=CARTESIAN_POINT('Ctrl Pts',(12.6834994414517,1.83095754915284,0.938423566452776));
#14278=CARTESIAN_POINT('Ctrl Pts',(12.6812592544344,1.82871566395046,0.981053704089438));
#14279=CARTESIAN_POINT('Ctrl Pts',(12.6790190612712,1.82647376985122,1.02368384096639));
#14280=CARTESIAN_POINT('Ctrl Pts',(12.7096132738247,1.83593722009608,0.897188525535458));
#14281=CARTESIAN_POINT('Ctrl Pts',(12.7073735515623,1.83369637734113,0.939818742641338));
#14282=CARTESIAN_POINT('Ctrl Pts',(12.7051338254027,1.83145551796363,0.982448958687984));
#14283=CARTESIAN_POINT('Ctrl Pts',(12.7028940916787,1.82921465970329,1.02507917444001));
#14284=CARTESIAN_POINT('Ctrl Pts',(12.7586310095219,1.82964538228831,0.8994266592275));
#14285=CARTESIAN_POINT('Ctrl Pts',(12.7563927428119,1.82740607701793,0.942057032676437));
#14286=CARTESIAN_POINT('Ctrl Pts',(12.7541544559015,1.82516675428928,0.984687404166494));
#14287=CARTESIAN_POINT('Ctrl Pts',(12.7519161806021,1.82292743696394,1.02731777659207));
#14288=CARTESIAN_POINT('Ctrl Pts',(12.8300025526753,1.78023902864912,0.90056967297836));
#14289=CARTESIAN_POINT('Ctrl Pts',(12.8277672375473,1.7780001144899,0.943200215636435));
#14290=CARTESIAN_POINT('Ctrl Pts',(12.8255319263559,1.7757611919149,0.985830758073823));
#14291=CARTESIAN_POINT('Ctrl Pts',(12.8232966088089,1.77352226682369,1.02846130007111));
#14292=CARTESIAN_POINT('Ctrl Pts',(12.8529050075203,1.72043671272769,0.898625988813541));
#14293=CARTESIAN_POINT('Ctrl Pts',(12.8506708576607,1.71819639833573,0.941256511626846));
#14294=CARTESIAN_POINT('Ctrl Pts',(12.8484366444933,1.71595605563573,0.983887029620282));
#14295=CARTESIAN_POINT('Ctrl Pts',(12.8462024947189,1.71371572743615,1.0265175517275));
#14296=CARTESIAN_POINT('Ctrl Pts',(12.853004077605,1.68438049200639,0.896735618985435));
#14297=CARTESIAN_POINT('Ctrl Pts',(12.8507699092581,1.68213930602179,0.939366090596142));
#14298=CARTESIAN_POINT('Ctrl Pts',(12.8485357409326,1.67989811224666,0.981996561798403));
#14299=CARTESIAN_POINT('Ctrl Pts',(12.8463015726285,1.67765691065502,1.02462703259085));
#14300=CARTESIAN_POINT('',(12.8528329986453,1.6842088756636,0.9));
#14301=CARTESIAN_POINT('Ctrl Pts',(12.8463246402318,1.67768005087614,1.02418687649944));
#14302=CARTESIAN_POINT('Ctrl Pts',(12.8484940930161,1.67985633316752,0.982791251385616));
#14303=CARTESIAN_POINT('Ctrl Pts',(12.8506635458206,1.68203260808875,0.941395625885387));
#14304=CARTESIAN_POINT('Ctrl Pts',(12.8528329986453,1.6842088756636,0.9));
#14305=CARTESIAN_POINT('Ctrl Pts',(12.8528329986453,1.6842088756636,0.900000000000001));
#14306=CARTESIAN_POINT('Ctrl Pts',(12.8528329990894,1.69496116035511,0.900000000031321));
#14307=CARTESIAN_POINT('Ctrl Pts',(12.8516279916809,1.7056415234076,0.899996564780585));
#14308=CARTESIAN_POINT('Ctrl Pts',(12.8493173682463,1.71608623918215,0.899994054968391));
#14309=CARTESIAN_POINT('Ctrl Pts',(12.847426586744,1.72463314262321,0.89999200119087));
#14310=CARTESIAN_POINT('Ctrl Pts',(12.8447941883809,1.73302290492875,0.899990534206534));
#14311=CARTESIAN_POINT('Ctrl Pts',(12.8414494901174,1.74115996769839,0.899990418365756));
#14312=CARTESIAN_POINT('Ctrl Pts',(12.8373567881217,1.75111679202539,0.899990276618506));
#14313=CARTESIAN_POINT('Ctrl Pts',(12.8322422209112,1.76059035368083,0.899992293328656));
#14314=CARTESIAN_POINT('Ctrl Pts',(12.8261823199623,1.76941466903515,0.899994578235276));
#14315=CARTESIAN_POINT('Ctrl Pts',(12.8228443945912,1.77427529404419,0.899995836811587));
#14316=CARTESIAN_POINT('Ctrl Pts',(12.819218773978,1.77893868154471,0.899997117508201));
#14317=CARTESIAN_POINT('Ctrl Pts',(12.8153125401773,1.78337342370743,0.899997612422461));
#14318=CARTESIAN_POINT('Ctrl Pts',(12.8134661485928,1.78546962967624,0.899997846357645));
#14319=CARTESIAN_POINT('Ctrl Pts',(12.8115570049875,1.7875146981109,0.899997899028016));
#14320=CARTESIAN_POINT('Ctrl Pts',(12.8095877759185,1.78950657520057,0.899997852068527));
#14321=CARTESIAN_POINT('Ctrl Pts',(12.802037518393,1.7971436679198,0.899997672020282));
#14322=CARTESIAN_POINT('Ctrl Pts',(12.7936869960543,1.80392089040634,0.899996345477631));
#14323=CARTESIAN_POINT('Ctrl Pts',(12.7847141304683,1.80975200096328,0.89999606036814));
#14324=CARTESIAN_POINT('Ctrl Pts',(12.7774211187199,1.81449144093269,0.899995828635385));
#14325=CARTESIAN_POINT('Ctrl Pts',(12.7697156358622,1.81860556854039,0.899996199361957));
#14326=CARTESIAN_POINT('Ctrl Pts',(12.761679297021,1.82202698480181,0.89999650903244));
#14327=CARTESIAN_POINT('Ctrl Pts',(12.7599722005109,1.82275376945776,0.899996574813315));
#14328=CARTESIAN_POINT('Ctrl Pts',(12.7582527406357,1.82344811243542,0.899996631272027));
#14329=CARTESIAN_POINT('Ctrl Pts',(12.7565217796305,1.82410952822173,0.899996662852262));
#14330=CARTESIAN_POINT('Ctrl Pts',(12.7461353325744,1.82807828316523,0.899996852346099));
#14331=CARTESIAN_POINT('Ctrl Pts',(12.7353361797362,1.83086624339127,0.899996468077086));
#14332=CARTESIAN_POINT('Ctrl Pts',(12.7243231747362,1.83245001845531,0.899997092905297));
#14333=CARTESIAN_POINT('Ctrl Pts',(12.713718016754,1.83397514123175,0.899997694594108));
#14334=CARTESIAN_POINT('Ctrl Pts',(12.702988146695,1.83437268605832,0.899999174299692));
#14335=CARTESIAN_POINT('Ctrl Pts',(12.6923097158784,1.83361665751845,0.899999788491474));
#14336=CARTESIAN_POINT('Ctrl Pts',(12.6900431251392,1.83345618381998,0.899999918859074));
#14337=CARTESIAN_POINT('Ctrl Pts',(12.6877788433122,1.83324355125563,0.900000000001074));
#14338=CARTESIAN_POINT('Ctrl Pts',(12.685518570211,1.83297820604925,0.9));
#14339=CARTESIAN_POINT('Origin',(6.88201982834292,-2.22044604925031E-16,
1.1));
#14340=CARTESIAN_POINT('Origin',(12.8528329986453,1.85283299864526,0.9));
#14341=CARTESIAN_POINT('',(12.8528329986453,-1.6842088756636,0.9));
#14342=CARTESIAN_POINT('Ctrl Pts',(12.8528329986453,-1.6842088756636,0.9));
#14343=CARTESIAN_POINT('Ctrl Pts',(12.8506635458206,-1.68203260808875,0.941395625885387));
#14344=CARTESIAN_POINT('Ctrl Pts',(12.8484940930161,-1.67985633316752,0.982791251385615));
#14345=CARTESIAN_POINT('Ctrl Pts',(12.8463246402318,-1.67768005087614,1.02418687649944));
#14346=CARTESIAN_POINT('',(12.8528329986453,1.85283299864526,0.9));
#14347=CARTESIAN_POINT('Ctrl Pts',(0.49319751180194,-1.1565009196418,0.896939762205254));
#14348=CARTESIAN_POINT('Ctrl Pts',(0.495422309889911,-1.15427605660646,
0.939415925341967));
#14349=CARTESIAN_POINT('Ctrl Pts',(0.49764710661353,-1.15205119483315,0.981892088611382));
#14350=CARTESIAN_POINT('Ctrl Pts',(0.499871901968411,-1.14982633432581,
1.02436825201392));
#14351=CARTESIAN_POINT('Ctrl Pts',(0.449154391250001,-1.15532331830903,
0.899186283506502));
#14352=CARTESIAN_POINT('Ctrl Pts',(0.451379443529967,-1.1530980743259,0.94166241338335));
#14353=CARTESIAN_POINT('Ctrl Pts',(0.453604490603533,-1.15087286444957,
0.984138545342204));
#14354=CARTESIAN_POINT('Ctrl Pts',(0.45582954070428,-1.14864762219213,1.02661467541392));
#14355=CARTESIAN_POINT('Ctrl Pts',(0.373709798968055,-1.1170292567097,0.901134386478875));
#14356=CARTESIAN_POINT('Ctrl Pts',(0.37593556973194,-1.11480381901192,0.943610469359475));
#14357=CARTESIAN_POINT('Ctrl Pts',(0.378161343437362,-1.11257837175868,
0.98608655157339));
#14358=CARTESIAN_POINT('Ctrl Pts',(0.380387113556173,-1.11035293539114,
1.02856263455032));
#14359=CARTESIAN_POINT('Ctrl Pts',(0.347087578105715,-1.039801123372,0.898484514129229));
#14360=CARTESIAN_POINT('Ctrl Pts',(0.349313658773859,-1.03757611304936,
0.940960604750146));
#14361=CARTESIAN_POINT('Ctrl Pts',(0.351539730193144,-1.03535109931323,
0.983436695671939));
#14362=CARTESIAN_POINT('Ctrl Pts',(0.353765810873703,-1.03312609123593,
1.02591278640767));
#14363=CARTESIAN_POINT('Ctrl Pts',(0.346997125389779,-1.00675922024802,
0.896758573492677));
#14364=CARTESIAN_POINT('Ctrl Pts',(0.349223203512402,-1.00453439127183,
0.939234674428006));
#14365=CARTESIAN_POINT('Ctrl Pts',(0.351449281638624,-1.0023095636104,0.98171077543201));
#14366=CARTESIAN_POINT('Ctrl Pts',(0.353675359768457,-1.00008473726791,
1.02418687650491));
#14367=CARTESIAN_POINT('',(0.493357799610228,-1.15634062715414,0.9));
#14368=CARTESIAN_POINT('Ctrl Pts',(0.347167001354737,-1.00658943961019,
0.900000000000001));
#14369=CARTESIAN_POINT('Ctrl Pts',(0.347167001425373,-1.01734828759763,
0.899999999998142));
#14370=CARTESIAN_POINT('Ctrl Pts',(0.348359077578701,-1.02805639415283,
0.899998433630397));
#14371=CARTESIAN_POINT('Ctrl Pts',(0.350656214310366,-1.0385309656087,0.899998024549738));
#14372=CARTESIAN_POINT('Ctrl Pts',(0.352533324612331,-1.04709028457193,
0.899997690268584));
#14373=CARTESIAN_POINT('Ctrl Pts',(0.355149562279486,-1.05549438497634,
0.899998101733499));
#14374=CARTESIAN_POINT('Ctrl Pts',(0.358482507184576,-1.0636377229308,0.899999127793999));
#14375=CARTESIAN_POINT('Ctrl Pts',(0.362555301547827,-1.07358872478153,
0.900000381620131));
#14376=CARTESIAN_POINT('Ctrl Pts',(0.367654000430903,-1.08304569392442,
0.900002668831236));
#14377=CARTESIAN_POINT('Ctrl Pts',(0.373714802804109,-1.09182534802447,
0.900002509451715));
#14378=CARTESIAN_POINT('Ctrl Pts',(0.375364773372187,-1.09421548879643,
0.90000246606282));
#14379=CARTESIAN_POINT('Ctrl Pts',(0.377086318771695,-1.09655531312597,
0.900002220932131));
#14380=CARTESIAN_POINT('Ctrl Pts',(0.378878733123435,-1.0988407769929,0.900001655250762));
#14381=CARTESIAN_POINT('Ctrl Pts',(0.382452759797804,-1.10339793132263,
0.900000527297116));
#14382=CARTESIAN_POINT('Ctrl Pts',(0.386308400219556,-1.10773917492176,
0.899998144709029));
#14383=CARTESIAN_POINT('Ctrl Pts',(0.390420886280218,-1.11185064093822,
0.899995523300098));
#14384=CARTESIAN_POINT('Ctrl Pts',(0.398040323803163,-1.11946818856709,
0.899990666466232));
#14385=CARTESIAN_POINT('Ctrl Pts',(0.406457812610252,-1.12621813960646,
0.899985292057237));
#14386=CARTESIAN_POINT('Ctrl Pts',(0.41549254786509,-1.13203603704298,0.899982834497606));
#14387=CARTESIAN_POINT('Ctrl Pts',(0.422749169000726,-1.13670892189372,
0.899980860606988));
#14388=CARTESIAN_POINT('Ctrl Pts',(0.430405328105449,-1.14078012415116,
0.899980677151631));
#14389=CARTESIAN_POINT('Ctrl Pts',(0.438380728308649,-1.14419607025517,
0.899982305341352));
#14390=CARTESIAN_POINT('Ctrl Pts',(0.448245442291908,-1.14842122892304,
0.899984319237269));
#14391=CARTESIAN_POINT('Ctrl Pts',(0.458495412124849,-1.1516012547891,0.899989147510445));
#14392=CARTESIAN_POINT('Ctrl Pts',(0.468969635281765,-1.1536564168707,0.899993562691215));
#14393=CARTESIAN_POINT('Ctrl Pts',(0.476989372009021,-1.15522998071208,
0.899996943236659));
#14394=CARTESIAN_POINT('Ctrl Pts',(0.485141446557615,-1.15614341614473,
0.89999999999177));
#14395=CARTESIAN_POINT('Ctrl Pts',(0.493357799610229,-1.15634062715414,
0.9));
#14396=CARTESIAN_POINT('Ctrl Pts',(0.493357799610229,-1.15634062715414,
0.9));
#14397=CARTESIAN_POINT('Ctrl Pts',(0.495527690583772,-1.1541706728313,0.941427869885423));
#14398=CARTESIAN_POINT('Ctrl Pts',(0.497697580259374,-1.15200071970906,
0.982855739897088));
#14399=CARTESIAN_POINT('Ctrl Pts',(0.499867468632967,-1.14983076779109,
1.02428361003538));
#14400=CARTESIAN_POINT('Ctrl Pts',(12.8530083952718,-1.68438482323521,0.896653232994753));
#14401=CARTESIAN_POINT('Ctrl Pts',(12.8507727877026,-1.68214219351771,0.939311166602882));
#14402=CARTESIAN_POINT('Ctrl Pts',(12.8485371801548,-1.67989955599965,0.98196909980204));
#14403=CARTESIAN_POINT('Ctrl Pts',(12.8463015726285,-1.67765691065502,1.02462703259086));
#14404=CARTESIAN_POINT('Ctrl Pts',(12.852942348552,-1.70842230260233,0.897913479482771));
#14405=CARTESIAN_POINT('Ctrl Pts',(12.8507067417858,-1.70618025058462,0.940571446443912));
#14406=CARTESIAN_POINT('Ctrl Pts',(12.8484711274102,-1.70393818829512,0.983229412467123));
#14407=CARTESIAN_POINT('Ctrl Pts',(12.8462355206888,-1.70169612184244,1.02588737868196));
#14408=CARTESIAN_POINT('Ctrl Pts',(12.8409786353997,-1.75638702494578,0.899808108153313));
#14409=CARTESIAN_POINT('Ctrl Pts',(12.838742445636,-1.75414612041198,0.942466110756886));
#14410=CARTESIAN_POINT('Ctrl Pts',(12.8365062537503,-1.75190518941781,0.985124111849326));
#14411=CARTESIAN_POINT('Ctrl Pts',(12.8342700627828,-1.74966427281549,1.02778211378599));
#14412=CARTESIAN_POINT('Ctrl Pts',(12.7836010260412,-1.82153168011476,0.900225885582409));
#14413=CARTESIAN_POINT('Ctrl Pts',(12.7813622549889,-1.8192914414386,0.942883795866658));
#14414=CARTESIAN_POINT('Ctrl Pts',(12.7791234760524,-1.81705120036295,0.985541705643422));
#14415=CARTESIAN_POINT('Ctrl Pts',(12.7768846983302,-1.81481095080325,1.02819961506361));
#14416=CARTESIAN_POINT('Ctrl Pts',(12.7215544275214,-1.83731044697508,0.89780368869924));
#14417=CARTESIAN_POINT('Ctrl Pts',(12.7193134882941,-1.83506869652207,0.940461407834127));
#14418=CARTESIAN_POINT('Ctrl Pts',(12.7170725571902,-1.83282686943458,0.983119123314088));
#14419=CARTESIAN_POINT('Ctrl Pts',(12.7148316068824,-1.83058510462933,1.02577684117682));
#14420=CARTESIAN_POINT('Ctrl Pts',(12.6857439516282,-1.83320375805174,0.895711042712126));
#14421=CARTESIAN_POINT('Ctrl Pts',(12.6835023276506,-1.83096043753957,0.938368642889274));
#14422=CARTESIAN_POINT('Ctrl Pts',(12.6812606975378,-1.82871710814956,0.981026242308181));
#14423=CARTESIAN_POINT('Ctrl Pts',(12.6790190612712,-1.82647376985122,1.02368384096639));
#14424=CARTESIAN_POINT('',(12.685518570211,-1.83297820604925,0.9));
#14425=CARTESIAN_POINT('Ctrl Pts',(12.6790190612712,-1.82647376985122,1.02368384096639));
#14426=CARTESIAN_POINT('Ctrl Pts',(12.6811855699938,-1.8286419235626,0.982455894687418));
#14427=CARTESIAN_POINT('Ctrl Pts',(12.6833520729681,-1.83081006895277,0.941227947697881));
#14428=CARTESIAN_POINT('Ctrl Pts',(12.685518570211,-1.83297820604925,0.9));
#14429=CARTESIAN_POINT('Ctrl Pts',(12.685518570211,-1.83297820604925,0.9));
#14430=CARTESIAN_POINT('Ctrl Pts',(12.6962007718831,-1.83423224573831,0.900000000027109));
#14431=CARTESIAN_POINT('Ctrl Pts',(12.7069522081469,-1.8342814865544,0.899996797888993));
#14432=CARTESIAN_POINT('Ctrl Pts',(12.7175986228217,-1.83320546389923,0.899994443686255));
#14433=CARTESIAN_POINT('Ctrl Pts',(12.7263221437181,-1.83232378622612,0.899992514685985));
#14434=CARTESIAN_POINT('Ctrl Pts',(12.7349759538105,-1.83068541925521,0.899991134073322));
#14435=CARTESIAN_POINT('Ctrl Pts',(12.7434612806603,-1.82830833949467,0.899991022249493));
#14436=CARTESIAN_POINT('Ctrl Pts',(12.7538268490808,-1.82540452879472,0.899990885646912));
#14437=CARTESIAN_POINT('Ctrl Pts',(12.7638319405548,-1.82143037312377,0.899992779825431));
#14438=CARTESIAN_POINT('Ctrl Pts',(12.7733027638617,-1.81644210162737,0.899994914291513));
#14439=CARTESIAN_POINT('Ctrl Pts',(12.7785122133597,-1.81369829070399,0.899996088359796));
#14440=CARTESIAN_POINT('Ctrl Pts',(12.7835598637901,-1.81064675361041,0.899997279965736));
#14441=CARTESIAN_POINT('Ctrl Pts',(12.7884138119185,-1.80729078554336,0.899997716205233));
#14442=CARTESIAN_POINT('Ctrl Pts',(12.7907292666901,-1.80568990476168,0.899997924302393));
#14443=CARTESIAN_POINT('Ctrl Pts',(12.7930005978609,-1.80401968744988,0.8999979548189));
#14444=CARTESIAN_POINT('Ctrl Pts',(12.7952253950699,-1.80228259226775,0.89999788947913));
#14445=CARTESIAN_POINT('Ctrl Pts',(12.8036908359575,-1.7956728767752,0.899997640858734));
#14446=CARTESIAN_POINT('Ctrl Pts',(12.8113954895597,-1.78816822909976,0.899996334032805));
#14447=CARTESIAN_POINT('Ctrl Pts',(12.818232559256,-1.77993499666286,0.899996088064289));
#14448=CARTESIAN_POINT('Ctrl Pts',(12.8237887404903,-1.77324421631459,0.899995888176659));
#14449=CARTESIAN_POINT('Ctrl Pts',(12.8287718252447,-1.76607091125846,0.899996310183797));
#14450=CARTESIAN_POINT('Ctrl Pts',(12.8331051219922,-1.75848815553817,0.899996624147351));
#14451=CARTESIAN_POINT('Ctrl Pts',(12.8340140186356,-1.75689769413573,0.899996690000312));
#14452=CARTESIAN_POINT('Ctrl Pts',(12.8348928881302,-1.75529157361675,0.899996744625968));
#14453=CARTESIAN_POINT('Ctrl Pts',(12.8357411680586,-1.75367056321155,0.89999677208873));
#14454=CARTESIAN_POINT('Ctrl Pts',(12.8409005734958,-1.74381125896804,0.89999693912265));
#14455=CARTESIAN_POINT('Ctrl Pts',(12.8449329422938,-1.7334030651393,0.899996442311536));
#14456=CARTESIAN_POINT('Ctrl Pts',(12.8477914282597,-1.72264121193733,0.899997037599541));
#14457=CARTESIAN_POINT('Ctrl Pts',(12.850541038206,-1.71228926375309,0.899997610213799));
#14458=CARTESIAN_POINT('Ctrl Pts',(12.8521849869391,-1.70168212150629,0.899999138466857));
#14459=CARTESIAN_POINT('Ctrl Pts',(12.8526768248801,-1.69099162083728,0.899999779783946));
#14460=CARTESIAN_POINT('Ctrl Pts',(12.8527806949164,-1.68873392048611,0.899999915222113));
#14461=CARTESIAN_POINT('Ctrl Pts',(12.8528329986625,-1.68647247255235,0.90000000000128));
#14462=CARTESIAN_POINT('Ctrl Pts',(12.8528329986453,-1.6842088756636,0.9));
#14463=CARTESIAN_POINT('Origin',(6.88173176806555,0.,0.9));
#14464=CARTESIAN_POINT('Ctrl Pts',(12.685518570211,-1.83297820604925,0.9));
#14465=CARTESIAN_POINT('Ctrl Pts',(8.62146498001073,-1.3558778793304,0.9));
#14466=CARTESIAN_POINT('Ctrl Pts',(4.55741138981048,-1.2538870134557,0.9));
#14467=CARTESIAN_POINT('Ctrl Pts',(0.493357799610228,-1.15634062715414,
0.9));
#14468=CARTESIAN_POINT('Ctrl Pts',(12.685518570211,-1.83297820604925,0.9));
#14469=CARTESIAN_POINT('Ctrl Pts',(12.6834055233574,-1.83080706336992,0.941427870232769));
#14470=CARTESIAN_POINT('Ctrl Pts',(12.6812924765039,-1.8286359206906,0.982855740465538));
#14471=CARTESIAN_POINT('Ctrl Pts',(12.6791794296503,-1.82646477801127,1.02428361069831));
#14472=CARTESIAN_POINT('Ctrl Pts',(8.62146498001072,-1.3558778793304,0.9));
#14473=CARTESIAN_POINT('Ctrl Pts',(8.62076307594679,-1.35370673665108,0.941427870232769));
#14474=CARTESIAN_POINT('Ctrl Pts',(8.62006117188285,-1.35153559397175,0.982855740465538));
#14475=CARTESIAN_POINT('Ctrl Pts',(8.61935926781891,-1.34936445129242,1.02428361069831));
#14476=CARTESIAN_POINT('Ctrl Pts',(4.55741138981048,-1.2538870134557,0.9));
#14477=CARTESIAN_POINT('Ctrl Pts',(4.55812062853616,-1.25171587077637,0.941427870232769));
#14478=CARTESIAN_POINT('Ctrl Pts',(4.55882986726185,-1.24954472809705,0.982855740465538));
#14479=CARTESIAN_POINT('Ctrl Pts',(4.55953910598754,-1.24737358541772,1.02428361069831));
#14480=CARTESIAN_POINT('Ctrl Pts',(0.493357799610228,-1.15634062715414,
0.9));
#14481=CARTESIAN_POINT('Ctrl Pts',(0.495478181125536,-1.15416948447481,
0.941427870232769));
#14482=CARTESIAN_POINT('Ctrl Pts',(0.497598562640844,-1.15199834179549,
0.982855740465538));
#14483=CARTESIAN_POINT('Ctrl Pts',(0.499718944156152,-1.14982719911616,
1.02428361069831));
#14484=CARTESIAN_POINT('',(0.,0.,0.));
#14485=CARTESIAN_POINT('Origin',(0.,0.,0.));
#14486=CARTESIAN_POINT('',(-0.14652705620645,9.44412402177196E-5,0.0160655045842905));
#14487=CARTESIAN_POINT('',(-0.146479946776166,0.000162062070299865,0.00893449541571059));
#14488=CARTESIAN_POINT('',(-0.14635,-1.79227059055215E-17,0.));
#14489=CARTESIAN_POINT('',(0.0634007094575209,0.131904027763685,0.));
#14490=CARTESIAN_POINT('Ctrl Pts',(-0.14652705620645,9.44412402177196E-5,
0.0160655045842905));
#14491=CARTESIAN_POINT('Ctrl Pts',(-0.146560923555419,0.00502618404349199,
0.0157963945919035));
#14492=CARTESIAN_POINT('Ctrl Pts',(-0.146333578783787,0.00995455679532004,
0.0155272845995164));
#14493=CARTESIAN_POINT('Ctrl Pts',(-0.14583475180505,0.0148550342388422,
0.0152581746071293));
#14494=CARTESIAN_POINT('Ctrl Pts',(-0.140929468554047,0.0630445487404258,
0.0126118447280274));
#14495=CARTESIAN_POINT('Ctrl Pts',(-0.10977174472993,0.108536575508351,
0.0099655148489255));
#14496=CARTESIAN_POINT('Ctrl Pts',(-0.0666135938566871,0.13056551637767,
0.00731918496982359));
#14497=CARTESIAN_POINT('Ctrl Pts',(-0.0268248419338395,0.150874636338504,
0.00487945664654906));
#14498=CARTESIAN_POINT('Ctrl Pts',(0.0231637104697219,0.151241233100125,
0.00243972832327453));
#14499=CARTESIAN_POINT('Ctrl Pts',(0.0635546915223951,0.132092229195826,
-2.16840434497101E-19));
#14500=CARTESIAN_POINT('',(-0.0634007094575146,0.131904027763688,0.));
#14501=CARTESIAN_POINT('Origin',(0.,0.,0.));
#14502=CARTESIAN_POINT('Ctrl Pts',(-0.0634007094575145,0.131904027763688,
-3.88578058618805E-16));
#14503=CARTESIAN_POINT('Ctrl Pts',(-0.107282641710421,0.110811831533068,
0.00264738937425961));
#14504=CARTESIAN_POINT('Ctrl Pts',(-0.139432201149969,0.0662847592091173,
0.00529477874851962));
#14505=CARTESIAN_POINT('Ctrl Pts',(-0.145436119191498,0.0182745223106641,
0.00794216812277962));
#14506=CARTESIAN_POINT('Ctrl Pts',(-0.146186273512714,0.0122759249909008,
0.00827294388708994));
#14507=CARTESIAN_POINT('Ctrl Pts',(-0.146528267289359,0.00622295186417552,
0.00860371965140026));
#14508=CARTESIAN_POINT('Ctrl Pts',(-0.146479946776166,0.000162062070299865,
0.00893449541571059));
#14509=CARTESIAN_POINT('Origin',(0.,0.,0.));
#14510=CARTESIAN_POINT('',(-0.146148830924315,7.59978318484386E-5,0.0660655045842905));
#14511=CARTESIAN_POINT('',(-0.146133770585873,6.2751561688711E-5,0.0589344954157103));
#14512=CARTESIAN_POINT('',(-0.14635,-1.79227059055215E-17,0.));
#14513=CARTESIAN_POINT('Ctrl Pts',(-0.146148830924315,7.59978318484386E-5,
0.0660655045842905));
#14514=CARTESIAN_POINT('Ctrl Pts',(-0.146240443598182,0.0195917497831913,
0.0650077071998482));
#14515=CARTESIAN_POINT('Ctrl Pts',(-0.142607114239671,0.0390747476468127,
0.0639499098154059));
#14516=CARTESIAN_POINT('Ctrl Pts',(-0.135087779856993,0.056920264102034,
0.0628921124309636));
#14517=CARTESIAN_POINT('Ctrl Pts',(-0.116276389754784,0.10156503643559,
0.0602457825518617));
#14518=CARTESIAN_POINT('Ctrl Pts',(-0.073143724514267,0.135961331060063,
0.0575994526727599));
#14519=CARTESIAN_POINT('Ctrl Pts',(-0.025432083612881,0.144366623974243,
0.054953122793658));
#14520=CARTESIAN_POINT('Ctrl Pts',(0.0222795572885053,0.152771916888423,
0.0523067929145561));
#14521=CARTESIAN_POINT('Ctrl Pts',(0.0745701738507606,0.135186208092309,
0.0496604630354541));
#14522=CARTESIAN_POINT('Ctrl Pts',(0.107505148494886,0.0996564726649905,
0.0470141331563522));
#14523=CARTESIAN_POINT('Ctrl Pts',(0.140440123139012,0.0641267372376721,
0.0443678032772503));
#14524=CARTESIAN_POINT('Ctrl Pts',(0.154019455865009,0.010652975179149,
0.0417214733981484));
#14525=CARTESIAN_POINT('Ctrl Pts',(0.14202839331759,-0.0362847016460775,
0.0390751435190465));
#14526=CARTESIAN_POINT('Ctrl Pts',(0.130037330770172,-0.0832223784713041,
0.0364288136399446));
#14527=CARTESIAN_POINT('Ctrl Pts',(0.0924758729493388,-0.123623970063234,
0.0337824837608427));
#14528=CARTESIAN_POINT('Ctrl Pts',(0.0465351214488668,-0.139005253038876,
0.0311361538817407));
#14529=CARTESIAN_POINT('Ctrl Pts',(0.000594369948394902,-0.154386536014517,
0.0284898240026388));
#14530=CARTESIAN_POINT('Ctrl Pts',(-0.0537256752317158,-0.144747510373871,
0.025843494123537));
#14531=CARTESIAN_POINT('Ctrl Pts',(-0.0915592764828275,-0.114484496435928,
0.0231971642444351));
#14532=CARTESIAN_POINT('Ctrl Pts',(-0.125545511528741,-0.0872989822136326,
0.0208199443577202));
#14533=CARTESIAN_POINT('Ctrl Pts',(-0.146227884351973,-0.0434707826450544,
0.0184427244710054));
#14534=CARTESIAN_POINT('Ctrl Pts',(-0.14652705620645,9.44412402177196E-5,
0.0160655045842905));
#14535=CARTESIAN_POINT('Ctrl Pts',(-0.146479946776166,0.000162062070299865,
0.00893449541571059));
#14536=CARTESIAN_POINT('Ctrl Pts',(-0.146141530330399,-0.0422858476614564,
0.0112511090256603));
#14537=CARTESIAN_POINT('Ctrl Pts',(-0.126658161292025,-0.0851220706608281,
0.0135677226356099));
#14538=CARTESIAN_POINT('Ctrl Pts',(-0.0941604943243988,-0.112386678841155,
0.0158843362455596));
#14539=CARTESIAN_POINT('Ctrl Pts',(-0.0570226747722624,-0.143544241621566,
0.0185317256198196));
#14540=CARTESIAN_POINT('Ctrl Pts',(-0.00288875902448078,-0.154365965709432,
0.0211791149940796));
#14541=CARTESIAN_POINT('Ctrl Pts',(0.0434083729543798,-0.140002007265973,
0.0238265043683396));
#14542=CARTESIAN_POINT('Ctrl Pts',(0.0897055049332404,-0.125638048822514,
0.0264738937425996));
#14543=CARTESIAN_POINT('Ctrl Pts',(0.12816585314318,-0.0860884078477292,
0.0291212831168596));
#14544=CARTESIAN_POINT('Ctrl Pts',(0.141191617966992,-0.0394144013492358,
0.0317686724911196));
#14545=CARTESIAN_POINT('Ctrl Pts',(0.154217382790803,0.00725960514925768,
0.0344160618653796));
#14546=CARTESIAN_POINT('Ctrl Pts',(0.141808564228487,0.0610579771714599,
0.0370634512396396));
#14547=CARTESIAN_POINT('Ctrl Pts',(0.109639063769471,0.0973098477439542,
0.0397108406138996));
#14548=CARTESIAN_POINT('Ctrl Pts',(0.0774695633104545,0.133561718316448,
0.0423582299881596));
#14549=CARTESIAN_POINT('Ctrl Pts',(0.0255393809547383,0.152267087439235,
0.0450056193624196));
#14550=CARTESIAN_POINT('Ctrl Pts',(-0.0223595433272462,0.144872892294413,
0.0476530087366796));
#14551=CARTESIAN_POINT('Ctrl Pts',(-0.070258467609231,0.137478697149591,
0.0503003981109396));
#14552=CARTESIAN_POINT('Ctrl Pts',(-0.114126133817484,0.10398493773716,
0.0529477874851996));
#14553=CARTESIAN_POINT('Ctrl Pts',(-0.133871661545403,0.059725601630819,
0.0555951768594596));
#14554=CARTESIAN_POINT('Ctrl Pts',(-0.142173753131161,0.0411165744656389,
0.0567082830448765));
#14555=CARTESIAN_POINT('Ctrl Pts',(-0.146211489678532,0.0206043892842972,
0.0578213892302934));
#14556=CARTESIAN_POINT('Ctrl Pts',(-0.146133770585873,6.2751561688711E-5,
0.0589344954157103));
#14557=CARTESIAN_POINT('Origin',(0.,0.,0.));
#14558=CARTESIAN_POINT('',(-0.146252097264499,-0.000124487410312429,0.116065504584291));
#14559=CARTESIAN_POINT('',(-0.146276374479508,-0.000129480650117819,0.10893449541571));
#14560=CARTESIAN_POINT('',(-0.14635,-1.79227059055215E-17,0.));
#14561=CARTESIAN_POINT('Ctrl Pts',(-0.146252097264499,-0.000124487410312429,
0.116065504584291));
#14562=CARTESIAN_POINT('Ctrl Pts',(-0.145977101830714,0.0338815411246725,
0.114219019807793));
#14563=CARTESIAN_POINT('Ctrl Pts',(-0.134160879762789,0.0680598926014691,
0.112372535031295));
#14564=CARTESIAN_POINT('Ctrl Pts',(-0.112484833627769,0.0939988017516943,
0.110526050254798));
#14565=CARTESIAN_POINT('Ctrl Pts',(-0.0814193359437304,0.131173714423195,
0.107879720375696));
#14566=CARTESIAN_POINT('Ctrl Pts',(-0.0301019434218634,0.151424966146533,
0.105233390496594));
#14567=CARTESIAN_POINT('Ctrl Pts',(0.0179785702873004,0.145483266051774,
0.102587060617492));
#14568=CARTESIAN_POINT('Ctrl Pts',(0.0660590839964643,0.139541565957016,
0.0999407307383904));
#14569=CARTESIAN_POINT('Ctrl Pts',(0.110902718892925,0.107406914044162,
0.0972944008592884));
#14570=CARTESIAN_POINT('Ctrl Pts',(0.131983829661647,0.0637877973597534,
0.0946480709801865));
#14571=CARTESIAN_POINT('Ctrl Pts',(0.15306494043037,0.0201686806753445,
0.0920017411010846));
#14572=CARTESIAN_POINT('Ctrl Pts',(0.150383527071356,-0.0349349007806195,
0.0893554112219828));
#14573=CARTESIAN_POINT('Ctrl Pts',(0.125166930059577,-0.0763010783846813,
0.0867090813428809));
#14574=CARTESIAN_POINT('Ctrl Pts',(0.0999503330477985,-0.117667255988743,
0.084062751463779));
#14575=CARTESIAN_POINT('Ctrl Pts',(0.0521985523832557,-0.145296029740903,
0.081416421584677));
#14576=CARTESIAN_POINT('Ctrl Pts',(0.00376830011669856,-0.146541450754272,
0.0787700917055751));
#14577=CARTESIAN_POINT('Ctrl Pts',(-0.0446619521498586,-0.147786871767642,
0.0761237618264732));
#14578=CARTESIAN_POINT('Ctrl Pts',(-0.09377067601843,-0.122648940042221,
0.0734774319473713));
#14579=CARTESIAN_POINT('Ctrl Pts',(-0.121079980470766,-0.0826333491581908,
0.0708311020682694));
#14580=CARTESIAN_POINT('Ctrl Pts',(-0.137473143648068,-0.0586128871159229,
0.0692425695736098));
#14581=CARTESIAN_POINT('Ctrl Pts',(-0.146011252866834,-0.02923151094855,
0.0676540370789502));
#14582=CARTESIAN_POINT('Ctrl Pts',(-0.146148830924315,7.59978318484386E-5,
0.0660655045842905));
#14583=CARTESIAN_POINT('Ctrl Pts',(-0.146133770585873,6.2751561688711E-5,
0.0589344954157103));
#14584=CARTESIAN_POINT('Ctrl Pts',(-0.146026644150963,-0.0282514289199324,
0.0604687786045534));
#14585=CARTESIAN_POINT('Ctrl Pts',(-0.138100435392092,-0.0566215672018456,
0.0620030617933965));
#14586=CARTESIAN_POINT('Ctrl Pts',(-0.122745086057252,-0.0801407530065182,
0.0635373449822396));
#14587=CARTESIAN_POINT('Ctrl Pts',(-0.0962495935935968,-0.120722858737265,
0.0661847343564996));
#14588=CARTESIAN_POINT('Ctrl Pts',(-0.0476352194187008,-0.146862157398507,
0.0688321237307596));
#14589=CARTESIAN_POINT('Ctrl Pts',(0.00082938917649622,-0.146587691816784,
0.0714795131050196));
#14590=CARTESIAN_POINT('Ctrl Pts',(0.0492939977716932,-0.146313226235061,
0.0741269024792796));
#14591=CARTESIAN_POINT('Ctrl Pts',(0.0976088407871913,-0.119624996410372,
0.0767742918535397));
#14592=CARTESIAN_POINT('Ctrl Pts',(0.123643642180798,-0.0787464320231966,
0.0794216812277997));
#14593=CARTESIAN_POINT('Ctrl Pts',(0.149678443574405,-0.0378678676360213,
0.0820690706020596));
#14594=CARTESIAN_POINT('Ctrl Pts',(0.153433203346121,0.0172010313136401,
0.0847164599763195));
#14595=CARTESIAN_POINT('Ctrl Pts',(0.133187835944515,0.06123527443138,0.0873638493505795));
#14596=CARTESIAN_POINT('Ctrl Pts',(0.11294246854291,0.10526951754912,0.0900112387248395));
#14597=CARTESIAN_POINT('Ctrl Pts',(0.0686969739679828,0.138269104834938,
0.0926586280990997));
#14598=CARTESIAN_POINT('Ctrl Pts',(0.0207181735233275,0.145118849380084,
0.0953060174733597));
#14599=CARTESIAN_POINT('Ctrl Pts',(-0.027260626921328,0.151968593925229,
0.0979534068476197));
#14600=CARTESIAN_POINT('Ctrl Pts',(-0.0789727332357116,0.132668495729702,
0.10060079622188));
#14601=CARTESIAN_POINT('Ctrl Pts',(-0.110731403441959,0.0960588230543748,
0.10324818559614));
#14602=CARTESIAN_POINT('Ctrl Pts',(-0.133469481440122,0.0698475998711364,
0.105143622202663));
#14603=CARTESIAN_POINT('Ctrl Pts',(-0.145979327216774,0.0347634013028336,
0.107039058809187));
#14604=CARTESIAN_POINT('Ctrl Pts',(-0.146276374479508,-0.000129480650117819,
0.10893449541571));
#14605=CARTESIAN_POINT('Origin',(0.,0.,0.));
#14606=CARTESIAN_POINT('',(-0.146589818999335,-3.81787486967988E-6,0.166065504584291));
#14607=CARTESIAN_POINT('',(-0.146589453522336,1.04004190909306E-5,0.15893449541571));
#14608=CARTESIAN_POINT('',(-0.14635,-1.79227059055215E-17,0.));
#14609=CARTESIAN_POINT('Ctrl Pts',(-0.146589818999335,-3.81787486967988E-6,
0.166065504584291));
#14610=CARTESIAN_POINT('Ctrl Pts',(-0.146571339149733,0.0482382848470949,
0.163430332415738));
#14611=CARTESIAN_POINT('Ctrl Pts',(-0.120433071521034,0.0964975486977609,
0.160795160247185));
#14612=CARTESIAN_POINT('Ctrl Pts',(-0.0800107885095625,0.122828684230981,
0.158159988078632));
#14613=CARTESIAN_POINT('Ctrl Pts',(-0.0394173515450545,0.149271309704865,
0.15551365819953));
#14614=CARTESIAN_POINT('Ctrl Pts',(0.0155813181737399,0.153599719825856,
0.152867328320428));
#14615=CARTESIAN_POINT('Ctrl Pts',(0.0598114643267532,0.133832733731537,
0.150220998441327));
#14616=CARTESIAN_POINT('Ctrl Pts',(0.104041610479766,0.114065747637217,
0.147574668562225));
#14617=CARTESIAN_POINT('Ctrl Pts',(0.137503233066998,0.0702033653275883,
0.144928338683123));
#14618=CARTESIAN_POINT('Ctrl Pts',(0.144880420813362,0.0223220882221681,
0.142282008804021));
#14619=CARTESIAN_POINT('Ctrl Pts',(0.152257608559726,-0.0255591888832524,
0.139635678924919));
#14620=CARTESIAN_POINT('Ctrl Pts',(0.133550361465222,-0.077459360784464,
0.136989349045817));
#14621=CARTESIAN_POINT('Ctrl Pts',(0.0973212811704284,-0.109622900294719,
0.134343019166715));
#14622=CARTESIAN_POINT('Ctrl Pts',(0.0610922008756344,-0.141786439804975,
0.131696689287613));
#14623=CARTESIAN_POINT('Ctrl Pts',(0.00734128738055008,-0.154213346924274,
0.129050359408511));
#14624=CARTESIAN_POINT('Ctrl Pts',(-0.0393288211819405,-0.141215634503184,
0.126404029529409));
#14625=CARTESIAN_POINT('Ctrl Pts',(-0.0859989297444312,-0.128217922082094,
0.123757699650308));
#14626=CARTESIAN_POINT('Ctrl Pts',(-0.125588233374328,-0.0897955901206149,
0.121111369771206));
#14627=CARTESIAN_POINT('Ctrl Pts',(-0.139976083766172,-0.043535137330043,
0.118465039892104));
#14628=CARTESIAN_POINT('Ctrl Pts',(-0.144324767489921,-0.0295530571287048,
0.117665194789499));
#14629=CARTESIAN_POINT('Ctrl Pts',(-0.146371217526823,-0.0148549394177889,
0.116865349686895));
#14630=CARTESIAN_POINT('Ctrl Pts',(-0.146252097264499,-0.000124487410312429,
0.116065504584291));
#14631=CARTESIAN_POINT('Ctrl Pts',(-0.146276374479508,-0.000129480650117819,
0.10893449541571));
#14632=CARTESIAN_POINT('Ctrl Pts',(-0.14639421831063,-0.0139720956278579,
0.109686448183447));
#14633=CARTESIAN_POINT('Ctrl Pts',(-0.14458995413065,-0.0277846002915201,
0.110438400951183));
#14634=CARTESIAN_POINT('Ctrl Pts',(-0.140739671041232,-0.041001045008257,
0.11119035371892));
#14635=CARTESIAN_POINT('Ctrl Pts',(-0.127184034336146,-0.0875319932404337,
0.11383774309318));
#14636=CARTESIAN_POINT('Ctrl Pts',(-0.0882675268278623,-0.12667464254966,
0.11648513246744));
#14637=CARTESIAN_POINT('Ctrl Pts',(-0.0418159243469935,-0.140499695546946,
0.1191325218417));
#14638=CARTESIAN_POINT('Ctrl Pts',(0.00463567813387508,-0.154324748544231,
0.12177991121596));
#14639=CARTESIAN_POINT('Ctrl Pts',(0.0586223755873289,-0.142832205229577,
0.12442730059022));
#14640=CARTESIAN_POINT('Ctrl Pts',(0.0954154960694136,-0.111286216216264,
0.12707468996448));
#14641=CARTESIAN_POINT('Ctrl Pts',(0.132208616551499,-0.0797402272029501,
0.12972207933874));
#14642=CARTESIAN_POINT('Ctrl Pts',(0.151808160062214,-0.0281407924909768,
0.132369468712999));
#14643=CARTESIAN_POINT('Ctrl Pts',(0.145236524363737,0.0198768833792122,
0.135016858087259));
#14644=CARTESIAN_POINT('Ctrl Pts',(0.138664888665259,0.0678945592494009,
0.13766424746152));
#14645=CARTESIAN_POINT('Ctrl Pts',(0.105922073757589,0.112330476277805,
0.14031163683578));
#14646=CARTESIAN_POINT('Ctrl Pts',(0.062005973158836,0.132830708741579,
0.14295902621004));
#14647=CARTESIAN_POINT('Ctrl Pts',(0.0180898725600832,0.153330941205352,
0.1456064155843));
#14648=CARTESIAN_POINT('Ctrl Pts',(-0.0369995137297515,0.149895489104495,
0.14825380495856));
#14649=CARTESIAN_POINT('Ctrl Pts',(-0.0780284182758478,0.124097962381086,
0.15090119433282));
#14650=CARTESIAN_POINT('Ctrl Pts',(-0.119057322821944,0.0983004356576776,
0.153548583707079));
#14651=CARTESIAN_POINT('Ctrl Pts',(-0.146025745624302,0.0501408343117172,
0.15619597308134));
#14652=CARTESIAN_POINT('Ctrl Pts',(-0.14658076309025,0.00167873146180186,
0.1588433624556));
#14653=CARTESIAN_POINT('Ctrl Pts',(-0.146587131676737,0.00112264969450139,
0.15887374010897));
#14654=CARTESIAN_POINT('Ctrl Pts',(-0.146590022522527,0.000566528098114988,
0.15890411776234));
#14655=CARTESIAN_POINT('Ctrl Pts',(-0.146589453522336,1.04004190909306E-5,
0.15893449541571));
#14656=CARTESIAN_POINT('Origin',(0.,0.,0.));
#14657=CARTESIAN_POINT('',(-0.146263250741535,0.000126870157254357,0.21606550458429));
#14658=CARTESIAN_POINT('',(-0.146245769975643,0.000123264779366826,0.20893449541571));
#14659=CARTESIAN_POINT('',(-0.14635,-1.79227059055215E-17,0.));
#14660=CARTESIAN_POINT('Ctrl Pts',(-0.146263250741535,0.000126870157254357,
0.21606550458429));
#14661=CARTESIAN_POINT('Ctrl Pts',(-0.146381923100139,0.0144435832128767,
0.215287974902784));
#14662=CARTESIAN_POINT('Ctrl Pts',(-0.144450237714319,0.0287289633064517,
0.214510445221278));
#14663=CARTESIAN_POINT('Ctrl Pts',(-0.140337374518256,0.0423560295890773,
0.213732915539772));
#14664=CARTESIAN_POINT('Ctrl Pts',(-0.126339204386259,0.0887358830222778,
0.21108658566067));
#14665=CARTESIAN_POINT('Ctrl Pts',(-0.0870745347363382,0.127489909020004,
0.208440255781569));
#14666=CARTESIAN_POINT('Ctrl Pts',(-0.0405154226099946,0.140879780169064,
0.205793925902467));
#14667=CARTESIAN_POINT('Ctrl Pts',(0.00604368951634975,0.154269651318124,
0.203147596023365));
#14668=CARTESIAN_POINT('Ctrl Pts',(0.0598972441191175,0.142295367618517,
0.200501266144263));
#14669=CARTESIAN_POINT('Ctrl Pts',(0.0963956219934077,0.110437747119808,
0.197854936265161));
#14670=CARTESIAN_POINT('Ctrl Pts',(0.132893999867697,0.0785801266211,0.195208606386059));
#14671=CARTESIAN_POINT('Ctrl Pts',(0.15203720101351,0.0268391693232909,
0.192562276506957));
#14672=CARTESIAN_POINT('Ctrl Pts',(0.145063081087281,-0.0211024746124516,
0.189915946627855));
#14673=CARTESIAN_POINT('Ctrl Pts',(0.138088961161051,-0.0690441185481943,
0.187269616748753));
#14674=CARTESIAN_POINT('Ctrl Pts',(0.10499752016278,-0.11318644912187,0.184623286869651));
#14675=CARTESIAN_POINT('Ctrl Pts',(0.060935231264163,-0.133324827106958,
0.181976956990549));
#14676=CARTESIAN_POINT('Ctrl Pts',(0.0168729423655461,-0.153463205092045,
0.179330627111448));
#14677=CARTESIAN_POINT('Ctrl Pts',(-0.0381601944334158,-0.149597630488544,
0.176684297232346));
#14678=CARTESIAN_POINT('Ctrl Pts',(-0.0789746466099193,-0.123497437688695,
0.174037967353244));
#14679=CARTESIAN_POINT('Ctrl Pts',(-0.119961184605052,-0.0972871987457574,
0.171380479763593));
#14680=CARTESIAN_POINT('Ctrl Pts',(-0.146608455341797,-0.0486544490602708,
0.168722992173942));
#14681=CARTESIAN_POINT('Ctrl Pts',(-0.146589818999335,-3.81787486967988E-6,
0.166065504584291));
#14682=CARTESIAN_POINT('Ctrl Pts',(-0.146589453522336,1.04004190909306E-5,
0.15893449541571));
#14683=CARTESIAN_POINT('Ctrl Pts',(-0.146540434588914,-0.0478995759235739,
0.1615515071366));
#14684=CARTESIAN_POINT('Ctrl Pts',(-0.120813506558866,-0.0958546957256878,
0.16416851885749));
#14685=CARTESIAN_POINT('Ctrl Pts',(-0.0808500697395765,-0.122278388912248,
0.16678553057838));
#14686=CARTESIAN_POINT('Ctrl Pts',(-0.0404227467934142,-0.149008802082514,
0.16943291995264));
#14687=CARTESIAN_POINT('Ctrl Pts',(0.0145735112284506,-0.153705024069172,
0.1720803093269));
#14688=CARTESIAN_POINT('Ctrl Pts',(0.0589475933459444,-0.134215943447351,
0.17472769870116));
#14689=CARTESIAN_POINT('Ctrl Pts',(0.103321675463438,-0.11472686282553,
0.17737508807542));
#14690=CARTESIAN_POINT('Ctrl Pts',(0.137073581676561,-0.0710524795952304,
0.18002247744968));
#14691=CARTESIAN_POINT('Ctrl Pts',(0.144743205110219,-0.0231979049720499,
0.18266986682394));
#14692=CARTESIAN_POINT('Ctrl Pts',(0.152412828543877,0.024656669651131,
0.1853172561982));
#14693=CARTESIAN_POINT('Ctrl Pts',(0.13400016919807,0.0766914356671922,
0.18796464557246));
#14694=CARTESIAN_POINT('Ctrl Pts',(0.0979391709064228,0.109071797518936,
0.19061203494672));
#14695=CARTESIAN_POINT('Ctrl Pts',(0.0618781726147763,0.141452159370678,
0.19325942432098));
#14696=CARTESIAN_POINT('Ctrl Pts',(0.00816883537729064,0.154178117058104,
0.195906813695239));
#14697=CARTESIAN_POINT('Ctrl Pts',(-0.0385872054932313,0.1414205281901,
0.198554203069499));
#14698=CARTESIAN_POINT('Ctrl Pts',(-0.0853432463637543,0.128662939322095,
0.201201592443759));
#14699=CARTESIAN_POINT('Ctrl Pts',(-0.125145990867313,0.0904218038986596,
0.20384898181802));
#14700=CARTESIAN_POINT('Ctrl Pts',(-0.139763737461459,0.0442135263146365,
0.20649637119228));
#14701=CARTESIAN_POINT('Ctrl Pts',(-0.144251162244238,0.030028291356252,
0.207309079266757));
#14702=CARTESIAN_POINT('Ctrl Pts',(-0.146365162502875,0.0150922359825044,
0.208121787341234));
#14703=CARTESIAN_POINT('Ctrl Pts',(-0.146245769975643,0.000123264779366826,
0.20893449541571));
#14704=CARTESIAN_POINT('Origin',(0.,0.,0.));
#14705=CARTESIAN_POINT('',(-0.146142672279203,-7.01165389862951E-5,0.266065504584291));
#14706=CARTESIAN_POINT('',(-0.146150215784492,-7.74481165901552E-5,0.258934495415711));
#14707=CARTESIAN_POINT('',(-0.14635,-1.79227059055215E-17,0.));
#14708=CARTESIAN_POINT('Ctrl Pts',(-0.146142672279203,-7.01165389862951E-5,
0.266065504584291));
#14709=CARTESIAN_POINT('Ctrl Pts',(-0.146017527260215,0.028828671850369,
0.264499287510729));
#14710=CARTESIAN_POINT('Ctrl Pts',(-0.137733916992107,0.0577936173630845,
0.262933070437168));
#14711=CARTESIAN_POINT('Ctrl Pts',(-0.121770841384076,0.0816117278206753,
0.261366853363607));
#14712=CARTESIAN_POINT('Ctrl Pts',(-0.0947991242083451,0.121855560193383,
0.258720523484505));
#14713=CARTESIAN_POINT('Ctrl Pts',(-0.0459036471244643,0.147405924851771,
0.256074193605403));
#14714=CARTESIAN_POINT('Ctrl Pts',(0.0025353607453442,0.146568017913755,
0.253427863726301));
#14715=CARTESIAN_POINT('Ctrl Pts',(0.050974368615152,0.145730110975738,
0.250781533847199));
#14716=CARTESIAN_POINT('Ctrl Pts',(0.0989569072708876,0.118503932441319,
0.248135203968097));
#14717=CARTESIAN_POINT('Ctrl Pts',(0.124520613871998,0.0773513325689396,
0.245488874088995));
#14718=CARTESIAN_POINT('Ctrl Pts',(0.150084320473109,0.0361987326965595,
0.242842544209893));
#14719=CARTESIAN_POINT('Ctrl Pts',(0.153229195019594,-0.0188802885137813,
0.240196214330791));
#14720=CARTESIAN_POINT('Ctrl Pts',(0.132515778953886,-0.0626751965094481,
0.237549884451689));
#14721=CARTESIAN_POINT('Ctrl Pts',(0.111802362888177,-0.106470104505115,
0.234903554572587));
#14722=CARTESIAN_POINT('Ctrl Pts',(0.0672306562102751,-0.138980899286108,
0.232257224693486));
#14723=CARTESIAN_POINT('Ctrl Pts',(0.0192018303028616,-0.145326878595667,
0.229610894814384));
#14724=CARTESIAN_POINT('Ctrl Pts',(-0.0288269956045516,-0.151672857905225,
0.226964564935282));
#14725=CARTESIAN_POINT('Ctrl Pts',(-0.0803129407414762,-0.131854021743351,
0.22431823505618));
#14726=CARTESIAN_POINT('Ctrl Pts',(-0.111690078002902,-0.0949417632280756,
0.221671905177078));
#14727=CARTESIAN_POINT('Ctrl Pts',(-0.133848162215005,-0.0688748557907962,
0.219803104979482));
#14728=CARTESIAN_POINT('Ctrl Pts',(-0.145978020566425,-0.0342834897603843,
0.217934304781886));
#14729=CARTESIAN_POINT('Ctrl Pts',(-0.146263250741535,0.000126870157254357,
0.21606550458429));
#14730=CARTESIAN_POINT('Ctrl Pts',(-0.146245769975643,0.000123264779366826,
0.20893449541571));
#14731=CARTESIAN_POINT('Ctrl Pts',(-0.145976242399967,-0.03366905549635,
0.210769176715493));
#14732=CARTESIAN_POINT('Ctrl Pts',(-0.134324750276972,-0.067629123606452,
0.212603858015276));
#14733=CARTESIAN_POINT('Ctrl Pts',(-0.112902327433,-0.0934976078712483,
0.214438539315059));
#14734=CARTESIAN_POINT('Ctrl Pts',(-0.0819904221256615,-0.130825044728502,
0.217085928689319));
#14735=CARTESIAN_POINT('Ctrl Pts',(-0.0307338628262512,-0.151304498698398,
0.21973331806358));
#14736=CARTESIAN_POINT('Ctrl Pts',(0.0173892134168267,-0.145555327884408,
0.22238070743784));
#14737=CARTESIAN_POINT('Ctrl Pts',(0.0655122896599044,-0.139806157070418,
0.2250280968121));
#14738=CARTESIAN_POINT('Ctrl Pts',(0.11050188284665,-0.107828361472542,
0.22767548618636));
#14739=CARTESIAN_POINT('Ctrl Pts',(0.131750448317205,-0.0642694140823833,
0.23032287556062));
#14740=CARTESIAN_POINT('Ctrl Pts',(0.15299901378776,-0.020710466692225,
0.232970264934879));
#14741=CARTESIAN_POINT('Ctrl Pts',(0.150506551542124,0.0344296324902152,
0.23561765430914));
#14742=CARTESIAN_POINT('Ctrl Pts',(0.125414737320077,0.0758938856636754,
0.2382650436834));
#14743=CARTESIAN_POINT('Ctrl Pts',(0.10032292309803,0.117358138837136,0.24091243305766));
#14744=CARTESIAN_POINT('Ctrl Pts',(0.0526317568995709,0.145146546001616,
0.24355982243192));
#14745=CARTESIAN_POINT('Ctrl Pts',(0.00418624259284972,0.146530589268381,
0.24620721180618));
#14746=CARTESIAN_POINT('Ctrl Pts',(-0.0442592717138715,0.147914632535146,
0.24885460118044));
#14747=CARTESIAN_POINT('Ctrl Pts',(-0.0934591341288551,0.122894311904195,
0.2515019905547));
#14748=CARTESIAN_POINT('Ctrl Pts',(-0.120877280418781,0.082930219442967,
0.25414937992896));
#14749=CARTESIAN_POINT('Ctrl Pts',(-0.137396572682769,0.0588520590724165,
0.255744418424543));
#14750=CARTESIAN_POINT('Ctrl Pts',(-0.146009100715185,0.0293493086505574,
0.257339456920127));
#14751=CARTESIAN_POINT('Ctrl Pts',(-0.146150215784492,-7.74481165901552E-5,
0.258934495415711));
#14752=CARTESIAN_POINT('Origin',(0.,0.,0.));
#14753=CARTESIAN_POINT('',(-0.146519404976022,-8.97763884284003E-5,0.316065504584291));
#14754=CARTESIAN_POINT('',(-0.146528765763263,-8.45393868379275E-5,0.30893449541571));
#14755=CARTESIAN_POINT('',(-0.14635,-1.79227059055215E-17,0.));
#14756=CARTESIAN_POINT('Ctrl Pts',(-0.146519404976022,-8.97763884284003E-5,
0.316065504584291));
#14757=CARTESIAN_POINT('Ctrl Pts',(-0.146208092107557,0.043076445171776,
0.313710600118674));
#14758=CARTESIAN_POINT('Ctrl Pts',(-0.125958424314353,0.0864965766126209,
0.311355695653057));
#14759=CARTESIAN_POINT('Ctrl Pts',(-0.0925183485457987,0.1137056160074,
0.309000791187441));
#14760=CARTESIAN_POINT('Ctrl Pts',(-0.0549399784004991,0.144281843189175,
0.306354461308339));
#14761=CARTESIAN_POINT('Ctrl Pts',(-0.00070450021881692,0.154386382754941,
0.303708131429237));
#14762=CARTESIAN_POINT('Ctrl Pts',(0.0453636543616171,0.139394227973128,
0.301061801550135));
#14763=CARTESIAN_POINT('Ctrl Pts',(0.0914318089420511,0.124402073191315,
0.298415471671033));
#14764=CARTESIAN_POINT('Ctrl Pts',(0.129332639921237,0.0843132240619223,
0.295769141791931));
#14765=CARTESIAN_POINT('Ctrl Pts',(0.141718340675246,0.0374769775398043,
0.293122811912829));
#14766=CARTESIAN_POINT('Ctrl Pts',(0.154104041429255,-0.00935926898231351,
0.290476482033727));
#14767=CARTESIAN_POINT('Ctrl Pts',(0.140974611958088,-0.0629429128971569,
0.287830152154626));
#14768=CARTESIAN_POINT('Ctrl Pts',(0.108339598692885,-0.0987478773661917,
0.285183822275524));
#14769=CARTESIAN_POINT('Ctrl Pts',(0.0757045854276824,-0.134552841835227,
0.282537492396422));
#14770=CARTESIAN_POINT('Ctrl Pts',(0.0235639883684441,-0.152579126858453,
0.27989116251732));
#14771=CARTESIAN_POINT('Ctrl Pts',(-0.0242166208952047,-0.144575818177467,
0.277244832638218));
#14772=CARTESIAN_POINT('Ctrl Pts',(-0.0719972301588528,-0.136572509496481,
0.274598502759116));
#14773=CARTESIAN_POINT('Ctrl Pts',(-0.115417851626912,-0.102539607111283,
0.271952172880014));
#14774=CARTESIAN_POINT('Ctrl Pts',(-0.13460418372715,-0.0580545058751705,
0.269305843000912));
#14775=CARTESIAN_POINT('Ctrl Pts',(-0.142435181350113,-0.0398976888130428,
0.268225730195372));
#14776=CARTESIAN_POINT('Ctrl Pts',(-0.146228976240411,-0.0199996345674016,
0.267145617389831));
#14777=CARTESIAN_POINT('Ctrl Pts',(-0.146142672279203,-7.01165389862951E-5,
0.266065504584291));
#14778=CARTESIAN_POINT('Ctrl Pts',(-0.146150215784492,-7.74481165901552E-5,
0.258934495415711));
#14779=CARTESIAN_POINT('Ctrl Pts',(-0.146243318595233,-0.0194921979337541,
0.259986846294387));
#14780=CARTESIAN_POINT('Ctrl Pts',(-0.142648899141753,-0.0388738684647463,
0.261039197173063));
#14781=CARTESIAN_POINT('Ctrl Pts',(-0.135204796371803,-0.0566427511368837,
0.26209154805174));
#14782=CARTESIAN_POINT('Ctrl Pts',(-0.116477735870028,-0.101343764964001,
0.264738937426));
#14783=CARTESIAN_POINT('Ctrl Pts',(-0.0733871847016099,-0.135837928326728,
0.26738632680026));
#14784=CARTESIAN_POINT('Ctrl Pts',(-0.0256708287318585,-0.144325142544676,
0.27003371617452));
#14785=CARTESIAN_POINT('Ctrl Pts',(0.0220455272378925,-0.152812356762624,
0.27268110554878));
#14786=CARTESIAN_POINT('Ctrl Pts',(0.0743876880089763,-0.135292621835792,
0.27532849492304));
#14787=CARTESIAN_POINT('Ctrl Pts',(0.10738025529095,-0.0997908762961729,
0.2779758842973));
#14788=CARTESIAN_POINT('Ctrl Pts',(0.140372822572925,-0.0642891307565533,
0.280623273671559));
#14789=CARTESIAN_POINT('Ctrl Pts',(0.154015796365789,-0.010805374604146,
0.283270663045819));
#14790=CARTESIAN_POINT('Ctrl Pts',(0.142059993874458,0.0361620845457957,
0.285918052420079));
#14791=CARTESIAN_POINT('Ctrl Pts',(0.130104191383128,0.0831295436957373,
0.288565441794339));
#14792=CARTESIAN_POINT('Ctrl Pts',(0.0925496126076039,0.123580705843213,
0.291212831168599));
#14793=CARTESIAN_POINT('Ctrl Pts',(0.0465981836912963,0.138986860871753,
0.29386022054286));
#14794=CARTESIAN_POINT('Ctrl Pts',(0.000646754774988913,0.154393015900293,
0.296507609917119));
#14795=CARTESIAN_POINT('Ctrl Pts',(-0.0537015242821025,0.144754163809898,
0.29915499929138));
#14796=CARTESIAN_POINT('Ctrl Pts',(-0.0915523499663989,0.114485393976436,
0.30180238866564));
#14797=CARTESIAN_POINT('Ctrl Pts',(-0.125542580994678,0.0873038870745135,
0.30417975758233));
#14798=CARTESIAN_POINT('Ctrl Pts',(-0.146229051243382,0.0434861464246214,
0.30655712649902));
#14799=CARTESIAN_POINT('Ctrl Pts',(-0.146528765763263,-8.45393868379275E-5,
0.30893449541571));
#14800=CARTESIAN_POINT('Origin',(0.,0.,0.));
#14801=CARTESIAN_POINT('',(-0.146416087288192,0.000126442170093593,0.366065504584291));
#14802=CARTESIAN_POINT('',(-0.146408012399712,0.000128195943346294,0.358934495415711));
#14803=CARTESIAN_POINT('',(-0.14635,-1.79227059055215E-17,0.));
#14804=CARTESIAN_POINT('Ctrl Pts',(-0.146416087288192,0.000126442170093593,
0.366065504584291));
#14805=CARTESIAN_POINT('Ctrl Pts',(-0.146499294961499,0.00925816812376314,
0.365568242605721));
#14806=CARTESIAN_POINT('Ctrl Pts',(-0.145718277739785,0.0183757049974218,
0.365070980627151));
#14807=CARTESIAN_POINT('Ctrl Pts',(-0.144021710151773,0.0273195705351122,
0.364573718648581));
#14808=CARTESIAN_POINT('Ctrl Pts',(-0.134992913071845,0.0749170536065741,
0.361927388769479));
#14809=CARTESIAN_POINT('Ctrl Pts',(-0.100034284522917,0.117595890322328,
0.359281058890377));
#14810=CARTESIAN_POINT('Ctrl Pts',(-0.0551469387876206,0.135821305661589,
0.356634729011275));
#14811=CARTESIAN_POINT('Ctrl Pts',(-0.0102595930523245,0.15404672100085,
0.353988399132173));
#14812=CARTESIAN_POINT('Ctrl Pts',(0.0445564698693406,0.147818714963618,
0.351342069253072));
#14813=CARTESIAN_POINT('Ctrl Pts',(0.0842110755700531,0.119987943896873,
0.34869573937397));
#14814=CARTESIAN_POINT('Ctrl Pts',(0.123865681270766,0.0921571728301272,
0.346049409494868));
#14815=CARTESIAN_POINT('Ctrl Pts',(0.148358829750526,0.0427236367338667,
0.343403079615766));
#14816=CARTESIAN_POINT('Ctrl Pts',(0.146479621605269,-0.00568615719458776,
0.340756749736664));
#14817=CARTESIAN_POINT('Ctrl Pts',(0.144600413460012,-0.0540959511230416,
0.338110419857562));
#14818=CARTESIAN_POINT('Ctrl Pts',(0.116348848689739,-0.101482002883689,
0.33546408997846));
#14819=CARTESIAN_POINT('Ctrl Pts',(0.0746561129649502,-0.126154971072205,
0.332817760099358));
#14820=CARTESIAN_POINT('Ctrl Pts',(0.0329633772401616,-0.150827939260721,
0.330171430220256));
#14821=CARTESIAN_POINT('Ctrl Pts',(-0.0221705294391424,-0.152787823877104,
0.327525100341154));
#14822=CARTESIAN_POINT('Ctrl Pts',(-0.0655099505772086,-0.131137554898038,
0.324878770462052));
#14823=CARTESIAN_POINT('Ctrl Pts',(-0.108849371715275,-0.109487285918972,
0.322232440582951));
#14824=CARTESIAN_POINT('Ctrl Pts',(-0.140394307312104,-0.0642268633444555,
0.319586110703849));
#14825=CARTESIAN_POINT('Ctrl Pts',(-0.14570614405606,-0.0160726946583056,
0.316939780824747));
#14826=CARTESIAN_POINT('Ctrl Pts',(-0.146291106736525,-0.0107697471190636,
0.316648355411261));
#14827=CARTESIAN_POINT('Ctrl Pts',(-0.146557930734812,-0.0054317060295066,
0.316356929997776));
#14828=CARTESIAN_POINT('Ctrl Pts',(-0.146519404976022,-8.97763884284003E-5,
0.316065504584291));
#14829=CARTESIAN_POINT('Ctrl Pts',(-0.146528765763263,-8.45393868379275E-5,
0.30893449541571));
#14830=CARTESIAN_POINT('Ctrl Pts',(-0.146562807199252,-0.00503327764821679,
0.30920451587328));
#14831=CARTESIAN_POINT('Ctrl Pts',(-0.14633385314783,-0.00997882882536714,
0.30947453633085));
#14832=CARTESIAN_POINT('Ctrl Pts',(-0.145831525524598,-0.0148964553326841,
0.309744556788419));
#14833=CARTESIAN_POINT('Ctrl Pts',(-0.140906503086998,-0.0631108472318147,
0.312391946162679));
#14834=CARTESIAN_POINT('Ctrl Pts',(-0.109703085900295,-0.108640943453547,
0.31503933553694));
#14835=CARTESIAN_POINT('Ctrl Pts',(-0.0665140418604196,-0.13063162118607,
0.3176867249112));
#14836=CARTESIAN_POINT('Ctrl Pts',(-0.0233249978205455,-0.152622298918592,
0.32033411428546));
#14837=CARTESIAN_POINT('Ctrl Pts',(0.0318496730725009,-0.151073558161906,
0.322981503659719));
#14838=CARTESIAN_POINT('Ctrl Pts',(0.0737371373950496,-0.126694801736668,
0.325628893033979));
#14839=CARTESIAN_POINT('Ctrl Pts',(0.115624601717599,-0.10231604531143,
0.328276282408239));
#14840=CARTESIAN_POINT('Ctrl Pts',(0.144224859469651,-0.0551072732176397,
0.3309236717825));
#14841=CARTESIAN_POINT('Ctrl Pts',(0.146437523492708,-0.0066925280449658,
0.33357106115676));
#14842=CARTESIAN_POINT('Ctrl Pts',(0.148650187515766,0.0417222171277085,
0.33621845053102));
#14843=CARTESIAN_POINT('Ctrl Pts',(0.124475257809829,0.0913429353792657,
0.33886583990528));
#14844=CARTESIAN_POINT('Ctrl Pts',(0.0849860939726622,0.119440788885456,
0.34151322927954));
#14845=CARTESIAN_POINT('Ctrl Pts',(0.0454969301354961,0.147538642391646,
0.344160618653799));
#14846=CARTESIAN_POINT('Ctrl Pts',(-0.00930646783289898,0.154113631152469,
0.346808008028059));
#14847=CARTESIAN_POINT('Ctrl Pts',(-0.0543213285795041,0.136154072578339,
0.349455397402319));
#14848=CARTESIAN_POINT('Ctrl Pts',(-0.0993361893261098,0.11819451400421,
0.352102786776579));
#14849=CARTESIAN_POINT('Ctrl Pts',(-0.134562512850926,0.0757004080951257,
0.35475017615084));
#14850=CARTESIAN_POINT('Ctrl Pts',(-0.143864833510727,0.0281362381501331,
0.3573975655251));
#14851=CARTESIAN_POINT('Ctrl Pts',(-0.145664973529558,0.0189318504589563,
0.357909875488637));
#14852=CARTESIAN_POINT('Ctrl Pts',(-0.146494308508217,0.00953759842677947,
0.358422185452174));
#14853=CARTESIAN_POINT('Ctrl Pts',(-0.146408012399712,0.000128195943346294,
0.358934495415711));
#14854=CARTESIAN_POINT('Origin',(0.,0.,0.));
#14855=CARTESIAN_POINT('',(-0.146110491840834,1.12683595067248E-5,0.416065504584291));
#14856=CARTESIAN_POINT('',(-0.146109756335714,8.81622270207575E-6,0.40893449541571));
#14857=CARTESIAN_POINT('',(-0.14635,-1.79227059055215E-17,0.));
#14858=CARTESIAN_POINT('Ctrl Pts',(-0.146110491840834,1.12683595067248E-5,
0.416065504584291));
#14859=CARTESIAN_POINT('Ctrl Pts',(-0.146126798292857,0.0237518011834032,
0.414779555213666));
#14860=CARTESIAN_POINT('Ctrl Pts',(-0.140669750958991,0.0474852665485293,
0.413493605843041));
#14861=CARTESIAN_POINT('Ctrl Pts',(-0.129698698951591,0.0683144158983218,
0.412207656472415));
#14862=CARTESIAN_POINT('Ctrl Pts',(-0.107121587134001,0.111178312051432,
0.409561326593314));
#14863=CARTESIAN_POINT('Ctrl Pts',(-0.0611933749717542,0.141742803557285,
0.406914996714211));
#14864=CARTESIAN_POINT('Ctrl Pts',(-0.0129361277491455,0.146018041789781,
0.40426866683511));
#14865=CARTESIAN_POINT('Ctrl Pts',(0.0353211194734639,0.150293280022276,
0.401622336956008));
#14866=CARTESIAN_POINT('Ctrl Pts',(0.0859074017564354,0.128279264981412,
0.398976007076906));
#14867=CARTESIAN_POINT('Ctrl Pts',(0.115668581836909,0.0900521576926538,
0.396329677197804));
#14868=CARTESIAN_POINT('Ctrl Pts',(0.145429761917382,0.0518250504038959,
0.393683347318702));
#14869=CARTESIAN_POINT('Ctrl Pts',(0.154365839795359,-0.0026151491327561,
0.3910370174396));
#14870=CARTESIAN_POINT('Ctrl Pts',(0.138386632036901,-0.0483503050946702,
0.388390687560498));
#14871=CARTESIAN_POINT('Ctrl Pts',(0.122407424278443,-0.094085461056585,
0.385744357681396));
#14872=CARTESIAN_POINT('Ctrl Pts',(0.0815129308835505,-0.131115573443762,
0.383098027802294));
#14873=CARTESIAN_POINT('Ctrl Pts',(0.0344212048624006,-0.142491377230642,
0.380451697923192));
#14874=CARTESIAN_POINT('Ctrl Pts',(-0.0126705211587486,-0.153867181017521,
0.37780536804409));
#14875=CARTESIAN_POINT('Ctrl Pts',(-0.0659594798061549,-0.139588676204105,
0.375159038164988));
#14876=CARTESIAN_POINT('Ctrl Pts',(-0.101054476324393,-0.106191359083811,
0.372512708285887));
#14877=CARTESIAN_POINT('Ctrl Pts',(-0.129554902927378,-0.0790696072742943,
0.370363640385355));
#14878=CARTESIAN_POINT('Ctrl Pts',(-0.146056480184715,-0.0393390709180539,
0.368214572484823));
#14879=CARTESIAN_POINT('Ctrl Pts',(-0.146416087288192,0.000126442170093593,
0.366065504584291));
#14880=CARTESIAN_POINT('Ctrl Pts',(-0.146408012399712,0.000128195943346294,
0.358934495415711));
#14881=CARTESIAN_POINT('Ctrl Pts',(-0.146048368712081,-0.0390859965171687,
0.361069574826434));
#14882=CARTESIAN_POINT('Ctrl Pts',(-0.1297855810823,-0.0785633296797545,
0.363204654237157));
#14883=CARTESIAN_POINT('Ctrl Pts',(-0.101613371150224,-0.105657280969165,
0.36533973364788));
#14884=CARTESIAN_POINT('Ctrl Pts',(-0.066681270335132,-0.139252396162569,
0.36798712302214));
#14885=CARTESIAN_POINT('Ctrl Pts',(-0.0134387509101597,-0.153808392568477,
0.370634512396399));
#14886=CARTESIAN_POINT('Ctrl Pts',(0.0337263783221333,-0.142657876135818,
0.373281901770659));
#14887=CARTESIAN_POINT('Ctrl Pts',(0.0808915075544263,-0.13150735970316,
0.375929291144919));
#14888=CARTESIAN_POINT('Ctrl Pts',(0.12197924659404,-0.0946503304319347,
0.378576680519179));
#14889=CARTESIAN_POINT('Ctrl Pts',(0.138169300408926,-0.0489692009616054,
0.38122406989344));
#14890=CARTESIAN_POINT('Ctrl Pts',(0.154359354223812,-0.00328807149127619,
0.3838714592677));
#14891=CARTESIAN_POINT('Ctrl Pts',(0.14565172281397,0.0512171581781573,
0.38651884864196));
#14892=CARTESIAN_POINT('Ctrl Pts',(0.11603494864959,0.0895802930905963,
0.38916623801622));
#14893=CARTESIAN_POINT('Ctrl Pts',(0.0864181744852101,0.127943428003035,
0.39181362739048));
#14894=CARTESIAN_POINT('Ctrl Pts',(0.0358922575662923,0.15016446815848,
0.394461016764739));
#14895=CARTESIAN_POINT('Ctrl Pts',(-0.0123993367959677,0.146065035738641,
0.397108406138999));
#14896=CARTESIAN_POINT('Ctrl Pts',(-0.0606909311582276,0.141965603318802,
0.399755795513259));
#14897=CARTESIAN_POINT('Ctrl Pts',(-0.106748202963829,0.111545698323679,
0.40240318488752));
#14898=CARTESIAN_POINT('Ctrl Pts',(-0.129474555904152,0.0687391998188283,
0.40505057426178));
#14899=CARTESIAN_POINT('Ctrl Pts',(-0.140588317483115,0.0478057390183907,
0.406345214646423));
#14900=CARTESIAN_POINT('Ctrl Pts',(-0.146122589096428,0.0239100770892618,
0.407639855031067));
#14901=CARTESIAN_POINT('Ctrl Pts',(-0.146109756335714,8.81622270207575E-6,
0.40893449541571));
#14902=CARTESIAN_POINT('Origin',(0.,0.,0.));
#14903=CARTESIAN_POINT('',(-0.146374718215768,-0.000132229735885947,0.466065504584291));
#14904=CARTESIAN_POINT('',(-0.146375609273197,-0.000132432188538665,0.458934495415711));
#14905=CARTESIAN_POINT('',(-0.14635,-1.79227059055215E-17,0.));
#14906=CARTESIAN_POINT('Ctrl Pts',(-0.146374718215768,-0.000132229735885947,
0.466065504584291));
#14907=CARTESIAN_POINT('Ctrl Pts',(-0.146022504084922,0.0379941335185874,
0.46399086782161));
#14908=CARTESIAN_POINT('Ctrl Pts',(-0.130761950520226,0.0763703265456945,
0.46191623105893));
#14909=CARTESIAN_POINT('Ctrl Pts',(-0.103994021541854,0.103314352404769,
0.45984159429625));
#14910=CARTESIAN_POINT('Ctrl Pts',(-0.0698498419286355,0.137683154682254,
0.457195264417148));
#14911=CARTESIAN_POINT('Ctrl Pts',(-0.0169824611430249,0.153451124186949,
0.454548934538046));
#14912=CARTESIAN_POINT('Ctrl Pts',(0.030409888879481,0.143401013202843,
0.451902604658944));
#14913=CARTESIAN_POINT('Ctrl Pts',(0.0778022389019875,0.133350902218736,
0.449256274779842));
#14914=CARTESIAN_POINT('Ctrl Pts',(0.119719558161389,0.0974827107458278,
0.44660994490074));
#14915=CARTESIAN_POINT('Ctrl Pts',(0.136975630157447,0.0522138743269898,
0.443963615021638));
#14916=CARTESIAN_POINT('Ctrl Pts',(0.154231702153504,0.00694503790815254,
0.441317285142536));
#14917=CARTESIAN_POINT('Ctrl Pts',(0.146826526886218,-0.0477244434566137,
0.438670955263434));
#14918=CARTESIAN_POINT('Ctrl Pts',(0.118149569579287,-0.0867714880447125,
0.436024625384332));
#14919=CARTESIAN_POINT('Ctrl Pts',(0.0894726122723542,-0.125818532632812,
0.43337829550523));
#14920=CARTESIAN_POINT('Ctrl Pts',(0.0395238729257754,-0.149243140444243,
0.430731965626129));
#14921=CARTESIAN_POINT('Ctrl Pts',(-0.00883432462988853,-0.146323499949933,
0.428085635747027));
#14922=CARTESIAN_POINT('Ctrl Pts',(-0.0571925221855517,-0.143403859455623,
0.425439305867925));
#14923=CARTESIAN_POINT('Ctrl Pts',(-0.1039601779503,-0.114139970655572,
0.422792975988823));
#14924=CARTESIAN_POINT('Ctrl Pts',(-0.127731000096207,-0.0719263758553634,
0.420146646109721));
#14925=CARTESIAN_POINT('Ctrl Pts',(-0.139950702323481,-0.0502259249733931,
0.418786265601244));
#14926=CARTESIAN_POINT('Ctrl Pts',(-0.146093241566443,-0.0251033736724598,
0.417425885092767));
#14927=CARTESIAN_POINT('Ctrl Pts',(-0.146110491840834,1.12683595067248E-5,
0.416065504584291));
#14928=CARTESIAN_POINT('Ctrl Pts',(-0.146109756335714,8.81622270207575E-6,
0.40893449541571));
#14929=CARTESIAN_POINT('Ctrl Pts',(-0.146096347589706,-0.0249652282079418,
0.410287244405327));
#14930=CARTESIAN_POINT('Ctrl Pts',(-0.140026707259891,-0.049945385460595,
0.411639993394943));
#14931=CARTESIAN_POINT('Ctrl Pts',(-0.127937780377622,-0.0715588049813403,
0.412992742384559));
#14932=CARTESIAN_POINT('Ctrl Pts',(-0.104279217835726,-0.113857219262079,
0.415640131758819));
#14933=CARTESIAN_POINT('Ctrl Pts',(-0.0575666586768896,-0.14326095580898,
0.41828752113308));
#14934=CARTESIAN_POINT('Ctrl Pts',(-0.00919685447762893,-0.146301592903247,
0.42093491050734));
#14935=CARTESIAN_POINT('Ctrl Pts',(0.039172949721632,-0.149342229997515,
0.4235822998816));
#14936=CARTESIAN_POINT('Ctrl Pts',(0.089199998961318,-0.126019767639148,
0.426229689255859));
#14937=CARTESIAN_POINT('Ctrl Pts',(0.117969334952632,-0.0870170915920772,
0.428877078630119));
#14938=CARTESIAN_POINT('Ctrl Pts',(0.146738670943946,-0.0480144155450057,
0.431524468004379));
#14939=CARTESIAN_POINT('Ctrl Pts',(0.154250293686888,0.00666847419077017,
0.43417185737864));
#14940=CARTESIAN_POINT('Ctrl Pts',(0.137063494116028,0.051984005222912,
0.4368192467529));
#14941=CARTESIAN_POINT('Ctrl Pts',(0.119876694545168,0.0972995362550541,
0.43946663612716));
#14942=CARTESIAN_POINT('Ctrl Pts',(0.0779914726605056,0.133247708583562,
0.442114025501419));
#14943=CARTESIAN_POINT('Ctrl Pts',(0.0305934116013849,0.143362412733947,
0.444761414875679));
#14944=CARTESIAN_POINT('Ctrl Pts',(-0.0168046494577345,0.153477116884331,
0.447408804249939));
#14945=CARTESIAN_POINT('Ctrl Pts',(-0.0697155496913122,0.137758352856595,
0.4500561936242));
#14946=CARTESIAN_POINT('Ctrl Pts',(-0.103903378920715,0.103406122000434,
0.45270358299846));
#14947=CARTESIAN_POINT('Ctrl Pts',(-0.130724942802416,0.0764555792150183,
0.45478055380421));
#14948=CARTESIAN_POINT('Ctrl Pts',(-0.146022533856355,0.0380362146017157,
0.45685752460996));
#14949=CARTESIAN_POINT('Ctrl Pts',(-0.146375609273197,-0.000132432188538665,
0.458934495415711));
#14950=CARTESIAN_POINT('Origin',(0.,0.,0.));
#14951=CARTESIAN_POINT('',(-0.146548608312775,6.99729089778146E-5,0.516065504584291));
#14952=CARTESIAN_POINT('',(-0.146550766805835,6.86360251013434E-5,0.508934495415711));
#14953=CARTESIAN_POINT('',(-0.14635,-1.79227059055215E-17,0.));
#14954=CARTESIAN_POINT('Ctrl Pts',(-0.146548608312775,6.99729089778146E-5,
0.516065504584291));
#14955=CARTESIAN_POINT('Ctrl Pts',(-0.146572081366671,0.00404546554386884,
0.515848510308657));
#14956=CARTESIAN_POINT('Ctrl Pts',(-0.146424333269732,0.00801918670503405,
0.515631516033023));
#14957=CARTESIAN_POINT('Ctrl Pts',(-0.146099725131082,0.0119784074854107,
0.51541452175739));
#14958=CARTESIAN_POINT('Ctrl Pts',(-0.142141002193345,0.06026265009261,
0.512768191878288));
#14959=CARTESIAN_POINT('Ctrl Pts',(-0.111878319621163,0.106390286678145,
0.510121861999186));
#14960=CARTESIAN_POINT('Ctrl Pts',(-0.069163383343408,0.129247972261684,
0.507475532120084));
#14961=CARTESIAN_POINT('Ctrl Pts',(-0.0264484470656534,0.152105657845224,
0.504829202240982));
#14962=CARTESIAN_POINT('Ctrl Pts',(0.0287187429176733,0.151693392426768,
0.50218287236188));
#14963=CARTESIAN_POINT('Ctrl Pts',(0.07108729581893,0.128199876374419,0.499536542482778));
#14964=CARTESIAN_POINT('Ctrl Pts',(0.113455848720186,0.10470636032207,0.496890212603677));
#14965=CARTESIAN_POINT('Ctrl Pts',(0.143025764539373,0.0581315936358261,
0.494243882724575));
#14966=CARTESIAN_POINT('Ctrl Pts',(0.146262427589597,0.00979357977770552,
0.491597552845473));
#14967=CARTESIAN_POINT('Ctrl Pts',(0.149499090639821,-0.0385444340804161,
0.488951222966371));
#14968=CARTESIAN_POINT('Ctrl Pts',(0.126402500921083,-0.0886456951104151,
0.486304893087269));
#14969=CARTESIAN_POINT('Ctrl Pts',(0.087544330920799,-0.117578067907642,
0.483658563208167));
#14970=CARTESIAN_POINT('Ctrl Pts',(0.0486861609205161,-0.146510440704867,
0.481012233329065));
#14971=CARTESIAN_POINT('Ctrl Pts',(-0.00593358936131212,-0.154273925269321,
0.478365903449963));
#14972=CARTESIAN_POINT('Ctrl Pts',(-0.0513146009011563,-0.137315052574797,
0.475719573570861));
#14973=CARTESIAN_POINT('Ctrl Pts',(-0.0966956124410008,-0.120356179880273,
0.473073243691759));
#14974=CARTESIAN_POINT('Ctrl Pts',(-0.132837885238862,-0.078674949926771,
0.470426913812657));
#14975=CARTESIAN_POINT('Ctrl Pts',(-0.14319853241738,-0.0313495174248821,
0.467780583933555));
#14976=CARTESIAN_POINT('Ctrl Pts',(-0.145436768368387,-0.0211256884885646,
0.467208890817134));
#14977=CARTESIAN_POINT('Ctrl Pts',(-0.146471775395962,-0.0106384445195334,
0.466637197700712));
#14978=CARTESIAN_POINT('Ctrl Pts',(-0.146374718215768,-0.000132229735885947,
0.466065504584291));
#14979=CARTESIAN_POINT('Ctrl Pts',(-0.146375609273197,-0.000132432188538665,
0.458934495415711));
#14980=CARTESIAN_POINT('Ctrl Pts',(-0.146472577787773,-0.0106150565970108,
0.45950491398422));
#14981=CARTESIAN_POINT('Ctrl Pts',(-0.145442327125792,-0.021078770125739,
0.46007533255273));
#14982=CARTESIAN_POINT('Ctrl Pts',(-0.143213999951756,-0.0312807998000163,
0.460645751121239));
#14983=CARTESIAN_POINT('Ctrl Pts',(-0.132872033528166,-0.0786297930597184,
0.463293140495499));
#14984=CARTESIAN_POINT('Ctrl Pts',(-0.0967233424557573,-0.120342081894533,
0.465940529869759));
#14985=CARTESIAN_POINT('Ctrl Pts',(-0.0513258840937604,-0.13731129538499,
0.46858791924402));
#14986=CARTESIAN_POINT('Ctrl Pts',(-0.00592842573176499,-0.154280508875447,
0.47123530861828));
#14987=CARTESIAN_POINT('Ctrl Pts',(0.0487177999198187,-0.146506647021548,
0.47388269799254));
#14988=CARTESIAN_POINT('Ctrl Pts',(0.0875820145025328,-0.117550537871965,
0.476530087366799));
#14989=CARTESIAN_POINT('Ctrl Pts',(0.126446229085248,-0.0885944287223814,
0.47917747674106));
#14990=CARTESIAN_POINT('Ctrl Pts',(0.149528432599094,-0.0384560722771122,
0.481824866115319));
#14991=CARTESIAN_POINT('Ctrl Pts',(0.146255790172295,0.0098985887573764,
0.484472255489579));
#14992=CARTESIAN_POINT('Ctrl Pts',(0.142983147745498,0.0582532497918637,
0.487119644863839));
#14993=CARTESIAN_POINT('Ctrl Pts',(0.113355659378058,0.10482421541557,0.4897670342381));
#14994=CARTESIAN_POINT('Ctrl Pts',(0.0709442366160257,0.128279591164298,
0.49241442361236));
#14995=CARTESIAN_POINT('Ctrl Pts',(0.0285328138539934,0.151734966913027,
0.49506181298662));
#14996=CARTESIAN_POINT('Ctrl Pts',(-0.0266625433026316,0.152074752786777,
0.497709202360879));
#14997=CARTESIAN_POINT('Ctrl Pts',(-0.0693595260588707,0.129143309401606,
0.500356591735139));
#14998=CARTESIAN_POINT('Ctrl Pts',(-0.11205650881511,0.106211866016435,
0.503003981109399));
#14999=CARTESIAN_POINT('Ctrl Pts',(-0.142255117170964,0.060009193372344,
0.505651370483659));
#15000=CARTESIAN_POINT('Ctrl Pts',(-0.146122837288996,0.0116984888307781,
0.50829875985792));
#15001=CARTESIAN_POINT('Ctrl Pts',(-0.146432431239741,0.00783142983325791,
0.508510671710517));
#15002=CARTESIAN_POINT('Ctrl Pts',(-0.14657331536999,0.00395086404934249,
0.508722583563114));
#15003=CARTESIAN_POINT('Ctrl Pts',(-0.146550766805835,6.86360251013434E-5,
0.508934495415711));
#15004=CARTESIAN_POINT('Origin',(0.,0.,0.));
#15005=CARTESIAN_POINT('',(-0.146165204287215,8.83645032875094E-5,0.566065504584291));
#15006=CARTESIAN_POINT('',(-0.146168951232552,9.12430751481418E-5,0.558934495415711));
#15007=CARTESIAN_POINT('',(-0.14635,-1.79227059055215E-17,0.));
#15008=CARTESIAN_POINT('Ctrl Pts',(-0.146165204287215,8.83645032875094E-5,
0.566065504584291));
#15009=CARTESIAN_POINT('Ctrl Pts',(-0.146267412293664,0.0186373661349918,
0.565059822916602));
#15010=CARTESIAN_POINT('Ctrl Pts',(-0.142994166834961,0.0371516370495788,
0.564054141248913));
#15011=CARTESIAN_POINT('Ctrl Pts',(-0.136179985035193,0.0542551712289143,
0.563048459581224));
#15012=CARTESIAN_POINT('Ctrl Pts',(-0.118249288396568,0.0992610562830057,
0.560402129702122));
#15013=CARTESIAN_POINT('Ctrl Pts',(-0.0758005933416487,0.134498778989873,
0.55775579982302));
#15014=CARTESIAN_POINT('Ctrl Pts',(-0.0282633354322908,0.143839479279877,
0.555109469943918));
#15015=CARTESIAN_POINT('Ctrl Pts',(0.0192739224770691,0.153180179569881,
0.552463140064816));
#15016=CARTESIAN_POINT('Ctrl Pts',(0.0718997432408687,0.136623857443018,
0.549816810185715));
#15017=CARTESIAN_POINT('Ctrl Pts',(0.105526460745998,0.101748602013432,
0.547170480306613));
#15018=CARTESIAN_POINT('Ctrl Pts',(0.139153178251127,0.0668733465838454,
0.544524150427511));
#15019=CARTESIAN_POINT('Ctrl Pts',(0.153780792497586,0.0136791578515372,
0.541877820548409));
#15020=CARTESIAN_POINT('Ctrl Pts',(0.142714014311998,-0.0334861471092027,
0.539231490669307));
#15021=CARTESIAN_POINT('Ctrl Pts',(0.13164723612641,-0.0806514520699426,
0.536585160790205));
#15022=CARTESIAN_POINT('Ctrl Pts',(0.0948860655087725,-0.121787873259113,
0.533938830911103));
#15023=CARTESIAN_POINT('Ctrl Pts',(0.0492566686055307,-0.138066623508903,
0.531292501032001));
#15024=CARTESIAN_POINT('Ctrl Pts',(0.00362727170228945,-0.154345373758693,
0.528646171152899));
#15025=CARTESIAN_POINT('Ctrl Pts',(-0.050870351486557,-0.145766453069103,
0.525999841273797));
#15026=CARTESIAN_POINT('Ctrl Pts',(-0.089291781429334,-0.116256568409877,
0.523353511394695));
#15027=CARTESIAN_POINT('Ctrl Pts',(-0.124562723435938,-0.0891664410515947,
0.520924175791227));
#15028=CARTESIAN_POINT('Ctrl Pts',(-0.146285818313441,-0.0444372186796531,
0.518494840187759));
#15029=CARTESIAN_POINT('Ctrl Pts',(-0.146548608312775,6.99729089778146E-5,
0.516065504584291));
#15030=CARTESIAN_POINT('Ctrl Pts',(-0.146550766805835,6.86360251013434E-5,
0.508934495415711));
#15031=CARTESIAN_POINT('Ctrl Pts',(-0.146291618860727,-0.0445493453248537,
0.511369972937373));
#15032=CARTESIAN_POINT('Ctrl Pts',(-0.124445252016267,-0.0893868858389474,
0.513805450459036));
#15033=CARTESIAN_POINT('Ctrl Pts',(-0.0890226177929609,-0.116463349340462,
0.516240927980699));
#15034=CARTESIAN_POINT('Ctrl Pts',(-0.0505178462986829,-0.145895746531099,
0.518888317354959));
#15035=CARTESIAN_POINT('Ctrl Pts',(0.00402852857008221,-0.154341804473332,
0.52153570672922));
#15036=CARTESIAN_POINT('Ctrl Pts',(0.0496314652424392,-0.137932794781367,
0.52418309610348));
#15037=CARTESIAN_POINT('Ctrl Pts',(0.0952344019147948,-0.121523785089403,
0.52683048547774));
#15038=CARTESIAN_POINT('Ctrl Pts',(0.131893900390741,-0.0802597077632436,
0.529477874851999));
#15039=CARTESIAN_POINT('Ctrl Pts',(0.14281802728161,-0.0330416298281342,
0.532125264226259));
#15040=CARTESIAN_POINT('Ctrl Pts',(0.153742154172479,0.0141764481069759,
0.53477265360052));
#15041=CARTESIAN_POINT('Ctrl Pts',(0.138930909478268,0.0673485266510362,
0.53742004297478));
#15042=CARTESIAN_POINT('Ctrl Pts',(0.105168604077417,0.102119062543277,
0.54006743234904));
#15043=CARTESIAN_POINT('Ctrl Pts',(0.0714062986765666,0.136889598435517,
0.5427148217233));
#15044=CARTESIAN_POINT('Ctrl Pts',(0.018692932569077,0.153258591675938,
0.545362211097559));
#15045=CARTESIAN_POINT('Ctrl Pts',(-0.0288260648428939,0.143728202535144,
0.548009600471819));
#15046=CARTESIAN_POINT('Ctrl Pts',(-0.0763450622548654,0.13419781339435,
0.550656989846079));
#15047=CARTESIAN_POINT('Ctrl Pts',(-0.118669690971318,0.0987680418723385,
0.55330437922034));
#15048=CARTESIAN_POINT('Ctrl Pts',(-0.136413096952957,0.0536675432455532,
0.5559517685946));
#15049=CARTESIAN_POINT('Ctrl Pts',(-0.143076734904351,0.036729792140314,
0.556946010868304));
#15050=CARTESIAN_POINT('Ctrl Pts',(-0.146273385252938,0.0184280612467595,
0.557940253142007));
#15051=CARTESIAN_POINT('Ctrl Pts',(-0.146168951232552,9.12430751481418E-5,
0.558934495415711));
#15052=CARTESIAN_POINT('Origin',(0.,0.,0.));
#15053=CARTESIAN_POINT('',(-0.146227179098081,-0.000117664897458569,0.616065504584291));
#15054=CARTESIAN_POINT('',(-0.146218520919543,-0.000115076211918358,0.608934495415711));
#15055=CARTESIAN_POINT('',(-0.14635,-1.79227059055215E-17,0.));
#15056=CARTESIAN_POINT('Ctrl Pts',(-0.146227179098081,-0.000117664897458569,
0.616065504584291));
#15057=CARTESIAN_POINT('Ctrl Pts',(-0.145977603365176,0.0329427899635141,
0.614271135524546));
#15058=CARTESIAN_POINT('Ctrl Pts',(-0.134874795495675,0.0661550248562671,
0.612476766464802));
#15059=CARTESIAN_POINT('Ctrl Pts',(-0.114309815624116,0.091770790457776,
0.610682397405058));
#15060=CARTESIAN_POINT('Ctrl Pts',(-0.0839806476072558,0.129548841477563,
0.608036067525956));
#15061=CARTESIAN_POINT('Ctrl Pts',(-0.0330710111925292,0.150804375664025,
0.605389737646855));
#15062=CARTESIAN_POINT('Ctrl Pts',(0.0151169520838501,0.145808400611758,
0.602743407767753));
#15063=CARTESIAN_POINT('Ctrl Pts',(0.0633049153602295,0.140812425559491,
0.600097077888651));
#15064=CARTESIAN_POINT('Ctrl Pts',(0.108771205498262,0.109564941268491,
0.597450748009549));
#15065=CARTESIAN_POINT('Ctrl Pts',(0.130705186191441,0.0663684129079872,
0.594804418130447));
#15066=CARTESIAN_POINT('Ctrl Pts',(0.152639166884621,0.023171884547483,
0.592158088251345));
#15067=CARTESIAN_POINT('Ctrl Pts',(0.151040838132949,-0.0319736878825246,
0.589511758372243));
#15068=CARTESIAN_POINT('Ctrl Pts',(0.126641780152193,-0.0738273082886534,
0.586865428493141));
#15069=CARTESIAN_POINT('Ctrl Pts',(0.102242722171437,-0.115680928694782,
0.584219098614039));
#15070=CARTESIAN_POINT('Ctrl Pts',(0.0550429349615966,-0.14424259707703,
0.581572768734937));
#15071=CARTESIAN_POINT('Ctrl Pts',(0.00664650371163741,-0.14643918846291,
0.578926438855836));
#15072=CARTESIAN_POINT('Ctrl Pts',(-0.0417499275383225,-0.148635779848789,
0.576280108976733));
#15073=CARTESIAN_POINT('Ctrl Pts',(-0.0913430028284016,-0.1244672942383,
0.573633779097631));
#15074=CARTESIAN_POINT('Ctrl Pts',(-0.119433191362276,-0.0849960277323969,
0.570987449218529));
#15075=CARTESIAN_POINT('Ctrl Pts',(-0.136848298201485,-0.0605249807527623,
0.569346801007117));
#15076=CARTESIAN_POINT('Ctrl Pts',(-0.145998464265635,-0.0301720919893573,
0.567706152795704));
#15077=CARTESIAN_POINT('Ctrl Pts',(-0.146165204287215,8.83645032875094E-5,
0.566065504584291));
#15078=CARTESIAN_POINT('Ctrl Pts',(-0.146168951232552,9.12430751481418E-5,
0.558934495415711));
#15079=CARTESIAN_POINT('Ctrl Pts',(-0.145995306636495,-0.0303977620653178,
0.560587642516267));
#15080=CARTESIAN_POINT('Ctrl Pts',(-0.136695352934655,-0.0609837708898569,
0.562240789616823));
#15081=CARTESIAN_POINT('Ctrl Pts',(-0.119031718004195,-0.0855580991331628,
0.563893936717379));
#15082=CARTESIAN_POINT('Ctrl Pts',(-0.090744749826965,-0.124912017153538,
0.566541326091639));
#15083=CARTESIAN_POINT('Ctrl Pts',(-0.0410086302256792,-0.148848627462727,
0.5691887154659));
#15084=CARTESIAN_POINT('Ctrl Pts',(0.00739494322942312,-0.146403732988417,
0.57183610484016));
#15085=CARTESIAN_POINT('Ctrl Pts',(0.0557985166845234,-0.143958838514108,
0.57448349421442));
#15086=CARTESIAN_POINT('Ctrl Pts',(0.10286954399344,-0.1151324392563,0.57713088358868));
#15087=CARTESIAN_POINT('Ctrl Pts',(0.127047076753504,-0.0731285067993286,
0.579778272962939));
#15088=CARTESIAN_POINT('Ctrl Pts',(0.151224609513568,-0.031124574342357,
0.5824256623372));
#15089=CARTESIAN_POINT('Ctrl Pts',(0.15250864772478,0.0240568913137802,
0.58507305171146));
#15090=CARTESIAN_POINT('Ctrl Pts',(0.130311035929276,0.0671399443948921,
0.58772044108572));
#15091=CARTESIAN_POINT('Ctrl Pts',(0.108113424133771,0.110222997476006,
0.59036783045998));
#15092=CARTESIAN_POINT('Ctrl Pts',(0.0624341623315493,0.141207637982093,
0.593015219834239));
#15093=CARTESIAN_POINT('Ctrl Pts',(0.0141966988324609,0.145901308974836,
0.595662609208499));
#15094=CARTESIAN_POINT('Ctrl Pts',(-0.0340407646666261,0.150594979967579,
0.598309998582759));
#15095=CARTESIAN_POINT('Ctrl Pts',(-0.0848364298625779,0.128997681446978,
0.60095738795702));
#15096=CARTESIAN_POINT('Ctrl Pts',(-0.114923272877171,0.091002085522857,
0.60360477733128));
#15097=CARTESIAN_POINT('Ctrl Pts',(-0.135113526827902,0.0655045372973676,
0.60538135002609));
#15098=CARTESIAN_POINT('Ctrl Pts',(-0.14597798884013,0.0326223532682757,
0.6071579227209));
#15099=CARTESIAN_POINT('Ctrl Pts',(-0.146218520919543,-0.000115076211918358,
0.608934495415711));
#15100=CARTESIAN_POINT('Origin',(0.,0.,0.));
#15101=CARTESIAN_POINT('',(-0.146586033401767,-2.15382961294558E-5,0.66606550458429));
#15102=CARTESIAN_POINT('',(-0.146582846697157,-3.00215943766004E-5,0.65893449541571));
#15103=CARTESIAN_POINT('',(-0.14635,-1.79227059055215E-17,0.));
#15104=CARTESIAN_POINT('Ctrl Pts',(-0.146586033401767,-2.15382961294558E-5,
0.66606550458429));
#15105=CARTESIAN_POINT('Ctrl Pts',(-0.146488810225965,0.0472697707580183,
0.663482448132491));
#15106=CARTESIAN_POINT('Ctrl Pts',(-0.121516563758978,0.0946492637554097,
0.660899391680692));
#15107=CARTESIAN_POINT('Ctrl Pts',(-0.0824084263440199,0.121233094478226,
0.658316335228893));
#15108=CARTESIAN_POINT('Ctrl Pts',(-0.0423423130056393,0.148468111155377,
0.655670005349791));
#15109=CARTESIAN_POINT('Ctrl Pts',(0.0125607065496858,0.153876184485078,
0.653023675470689));
#15110=CARTESIAN_POINT('Ctrl Pts',(0.0571706564953393,0.134981954220393,
0.650377345591587));
#15111=CARTESIAN_POINT('Ctrl Pts',(0.101780606440992,0.116087723955709,
0.647731015712485));
#15112=CARTESIAN_POINT('Ctrl Pts',(0.136097486776972,0.0728911900966409,
0.645084685833384));
#15113=CARTESIAN_POINT('Ctrl Pts',(0.144413921474191,0.0251640857912735,
0.642438355954282));
#15114=CARTESIAN_POINT('Ctrl Pts',(0.152730356171409,-0.0225630185140953,
0.63979202607518));
#15115=CARTESIAN_POINT('Ctrl Pts',(0.135046345229863,-0.0748206932657649,
0.637145696196077));
#15116=CARTESIAN_POINT('Ctrl Pts',(0.0994561386758346,-0.10768977857233,
0.634499366316975));
#15117=CARTESIAN_POINT('Ctrl Pts',(0.0638659321218069,-0.140558863878895,
0.631853036437873));
#15118=CARTESIAN_POINT('Ctrl Pts',(0.0103695299552984,-0.154039359740357,
0.629206706558772));
#15119=CARTESIAN_POINT('Ctrl Pts',(-0.0365469229059137,-0.141961031115491,
0.62656037667967));
#15120=CARTESIAN_POINT('Ctrl Pts',(-0.0834633757671259,-0.129882702490626,
0.623914046800568));
#15121=CARTESIAN_POINT('Ctrl Pts',(-0.123799879323041,-0.0922455493794331,
0.621267716921466));
#15122=CARTESIAN_POINT('Ctrl Pts',(-0.139093781291504,-0.0462766888972804,
0.618621387042364));
#15123=CARTESIAN_POINT('Ctrl Pts',(-0.14401750805555,-0.0314774500153124,
0.617769426223006));
#15124=CARTESIAN_POINT('Ctrl Pts',(-0.14634567687575,-0.0158146654998378,
0.616917465403648));
#15125=CARTESIAN_POINT('Ctrl Pts',(-0.146227179098081,-0.000117664897458569,
0.616065504584291));
#15126=CARTESIAN_POINT('Ctrl Pts',(-0.146218520919543,-0.000115076211918358,
0.608934495415711));
#15127=CARTESIAN_POINT('Ctrl Pts',(-0.1463364217222,-0.0161618722236638,
0.60980531209516));
#15128=CARTESIAN_POINT('Ctrl Pts',(-0.143901781624712,-0.032173889023867,
0.61067612877461));
#15129=CARTESIAN_POINT('Ctrl Pts',(-0.138761720114909,-0.0472643972675185,
0.611546945454059));
#15130=CARTESIAN_POINT('Ctrl Pts',(-0.123135303504819,-0.0931413908061287,
0.614194334828319));
#15131=CARTESIAN_POINT('Ctrl Pts',(-0.0825044494514074,-0.130501484555709,
0.616841724202579));
#15132=CARTESIAN_POINT('Ctrl Pts',(-0.0354801761942514,-0.142231836504824,
0.619489113576839));
#15133=CARTESIAN_POINT('Ctrl Pts',(0.0115440970629072,-0.15396218845394,
0.6221365029511));
#15134=CARTESIAN_POINT('Ctrl Pts',(0.0649617895238099,-0.140062798602586,
0.624783892325359));
#15135=CARTESIAN_POINT('Ctrl Pts',(0.100304854137336,-0.106900301471969,
0.627431281699619));
#15136=CARTESIAN_POINT('Ctrl Pts',(0.135647918750861,-0.0737378043413545,
0.630078671073879));
#15137=CARTESIAN_POINT('Ctrl Pts',(0.15291635551701,-0.0213121999314781,
0.63272606044814));
#15138=CARTESIAN_POINT('Ctrl Pts',(0.144200333369931,0.026362891994447,
0.6353734498224));
#15139=CARTESIAN_POINT('Ctrl Pts',(0.135484311222852,0.0740379839203748,
0.63802083919666));
#15140=CARTESIAN_POINT('Ctrl Pts',(0.100783830162543,0.11696256336235,0.640668228570919));
#15141=CARTESIAN_POINT('Ctrl Pts',(0.055993492972559,0.135474968031154,
0.643315617945179));
#15142=CARTESIAN_POINT('Ctrl Pts',(0.0112031557825773,0.153987372699956,
0.64596300731944));
#15143=CARTESIAN_POINT('Ctrl Pts',(-0.04367703753708,0.148087602595587,
0.6486103966937));
#15144=CARTESIAN_POINT('Ctrl Pts',(-0.0835091394177698,0.120478055479053,
0.65125778606796));
#15145=CARTESIAN_POINT('Ctrl Pts',(-0.122009894390588,0.0937913289882395,
0.653816689183877));
#15146=CARTESIAN_POINT('Ctrl Pts',(-0.146451680634158,0.0468218259492564,
0.656375592299793));
#15147=CARTESIAN_POINT('Ctrl Pts',(-0.146582846697157,-3.00215943766004E-5,
0.65893449541571));
#15148=CARTESIAN_POINT('Origin',(0.,0.,0.));
#15149=CARTESIAN_POINT('',(-0.146290249280603,0.000131112932912382,0.716065504584291));
#15150=CARTESIAN_POINT('',(-0.146307221518699,0.000133045872591754,0.708934495415711));
#15151=CARTESIAN_POINT('',(-0.14635,-1.79227059055215E-17,0.));
#15152=CARTESIAN_POINT('Ctrl Pts',(-0.146290249280603,0.000131112932912382,
0.716065504584291));
#15153=CARTESIAN_POINT('Ctrl Pts',(-0.146406294125046,0.0134819654399978,
0.715340090619538));
#15154=CARTESIAN_POINT('Ctrl Pts',(-0.144729088574721,0.0268041890186768,
0.714614676654786));
#15155=CARTESIAN_POINT('Ctrl Pts',(-0.141142411757643,0.0395908011096033,
0.713889262690033));
#15156=CARTESIAN_POINT('Ctrl Pts',(-0.128058117149462,0.0862367098911347,
0.711242932810931));
#15157=CARTESIAN_POINT('Ctrl Pts',(-0.0895623832093418,0.125754646095387,
0.708596602931829));
#15158=CARTESIAN_POINT('Ctrl Pts',(-0.0432753130058998,0.140056628595385,
0.705950273052727));
#15159=CARTESIAN_POINT('Ctrl Pts',(0.00301175719754219,0.154358611095384,
0.703303943173625));
#15160=CARTESIAN_POINT('Ctrl Pts',(0.0570901636643063,0.143444639891129,
0.700657613294523));
#15161=CARTESIAN_POINT('Ctrl Pts',(0.0942073689518517,0.11231021130972,
0.698011283415421));
#15162=CARTESIAN_POINT('Ctrl Pts',(0.131324574239397,0.0811757827283121,
0.695364953536319));
#15163=CARTESIAN_POINT('Ctrl Pts',(0.151480578347723,0.0298208967697505,
0.692718623657217));
#15164=CARTESIAN_POINT('Ctrl Pts',(0.145449661086834,-0.0182485073085286,
0.690072293778115));
#15165=CARTESIAN_POINT('Ctrl Pts',(0.139418743825945,-0.0663179113868083,
0.687425963899014));
#15166=CARTESIAN_POINT('Ctrl Pts',(0.107200905195838,-0.111101833584806,
0.684779634019911));
#15167=CARTESIAN_POINT('Ctrl Pts',(0.0635427568131047,-0.132101968137704,
0.68213330414081));
#15168=CARTESIAN_POINT('Ctrl Pts',(0.0198846084303716,-0.153102102690602,
0.679486974261708));
#15169=CARTESIAN_POINT('Ctrl Pts',(-0.0352138497049885,-0.150318449598402,
0.676840644382606));
#15170=CARTESIAN_POINT('Ctrl Pts',(-0.0765331864534889,-0.125025130675956,
0.674194314503504));
#15171=CARTESIAN_POINT('Ctrl Pts',(-0.117852523201989,-0.0997318117535095,
0.671547984624402));
#15172=CARTESIAN_POINT('Ctrl Pts',(-0.14539273856363,-0.0519288270008166,
0.6689016547453));
#15173=CARTESIAN_POINT('Ctrl Pts',(-0.146548242683733,-0.00349635461217019,
0.666255324866198));
#15174=CARTESIAN_POINT('Ctrl Pts',(-0.146575870647472,-0.00233834005587287,
0.666192051438896));
#15175=CARTESIAN_POINT('Ctrl Pts',(-0.146588414938392,-0.00117996563262623,
0.666128778011593));
#15176=CARTESIAN_POINT('Ctrl Pts',(-0.146586033401767,-2.15382961294558E-5,
0.66606550458429));
#15177=CARTESIAN_POINT('Ctrl Pts',(-0.146582846697157,-3.00215943766004E-5,
0.65893449541571));
#15178=CARTESIAN_POINT('Ctrl Pts',(-0.146587382388275,-0.00165014728799839,
0.659022981674053));
#15179=CARTESIAN_POINT('Ctrl Pts',(-0.146562848415234,-0.00327013229389975,
0.659111467932396));
#15180=CARTESIAN_POINT('Ctrl Pts',(-0.146508820881567,-0.00488913307276392,
0.659199954190739));
#15181=CARTESIAN_POINT('Ctrl Pts',(-0.144892390022949,-0.0533274503793473,
0.661847343564999));
#15182=CARTESIAN_POINT('Ctrl Pts',(-0.116875517863988,-0.100884760863813,
0.66449473293926));
#15183=CARTESIAN_POINT('Ctrl Pts',(-0.0752913709948059,-0.125777373450206,
0.66714212231352));
#15184=CARTESIAN_POINT('Ctrl Pts',(-0.0337072241256252,-0.150669986036599,
0.66978951168778));
#15185=CARTESIAN_POINT('Ctrl Pts',(0.021444197453776,-0.15289790072492,
0.672436901062039));
#15186=CARTESIAN_POINT('Ctrl Pts',(0.0649007096996251,-0.131440618146733,
0.675084290436299));
#15187=CARTESIAN_POINT('Ctrl Pts',(0.108357221945475,-0.109983335568545,
0.677731679810559));
#15188=CARTESIAN_POINT('Ctrl Pts',(0.140118824857774,-0.0648408557238465,
0.68037906918482));
#15189=CARTESIAN_POINT('Ctrl Pts',(0.145637072805965,-0.0166907532130915,
0.68302645855908));
#15190=CARTESIAN_POINT('Ctrl Pts',(0.151155320754156,0.031459349297663,
0.68567384793334));
#15191=CARTESIAN_POINT('Ctrl Pts',(0.130430213738242,0.0826170744744734,
0.688321237307599));
#15192=CARTESIAN_POINT('Ctrl Pts',(0.0929549153570804,0.113349556369966,
0.690968626681859));
#15193=CARTESIAN_POINT('Ctrl Pts',(0.0554796169759186,0.14408203826546,
0.693616016056119));
#15194=CARTESIAN_POINT('Ctrl Pts',(0.00125412722950909,0.154389276879634,
0.69626340543038));
#15195=CARTESIAN_POINT('Ctrl Pts',(-0.0448834941801804,0.139550027475769,
0.69891079480464));
#15196=CARTESIAN_POINT('Ctrl Pts',(-0.0910211155898686,0.124710778071904,
0.7015581841789));
#15197=CARTESIAN_POINT('Ctrl Pts',(-0.129070868662838,0.0847250406500019,
0.704205573553159));
#15198=CARTESIAN_POINT('Ctrl Pts',(-0.141604011991841,0.0379083368947344,
0.706852962927419));
#15199=CARTESIAN_POINT('Ctrl Pts',(-0.144888775625201,0.0256383259412015,
0.707546807090183));
#15200=CARTESIAN_POINT('Ctrl Pts',(-0.146420824649375,0.0128991016161637,
0.708240651252947));
#15201=CARTESIAN_POINT('Ctrl Pts',(-0.146307221518699,0.000133045872591754,
0.708934495415711));
#15202=CARTESIAN_POINT('Origin',(0.,0.,0.));
#15203=CARTESIAN_POINT('',(-0.1461301977291,-5.61458017395017E-5,0.766065504584291));
#15204=CARTESIAN_POINT('',(-0.14612241379348,-4.54149644099216E-5,0.758934495415711));
#15205=CARTESIAN_POINT('',(-0.14635,-1.79227059055215E-17,0.));
#15206=CARTESIAN_POINT('Ctrl Pts',(-0.1461301977291,-5.61458017395017E-5,
0.766065504584291));
#15207=CARTESIAN_POINT('Ctrl Pts',(-0.14603380141711,0.0278870014676159,
0.764551403227483));
#15208=CARTESIAN_POINT('Ctrl Pts',(-0.138327245009168,0.0558793842949389,
0.763037301870675));
#15209=CARTESIAN_POINT('Ctrl Pts',(-0.123350675409043,0.079203679241543,
0.761523200513867));
#15210=CARTESIAN_POINT('Ctrl Pts',(-0.0971747899961838,0.119969628197767,
0.758876870634766));
#15211=CARTESIAN_POINT('Ctrl Pts',(-0.048790709571801,0.146475657227381,
0.756230540755664));
#15212=CARTESIAN_POINT('Ctrl Pts',(-0.000344588961360588,0.146589539830481,
0.753584210876561));
#15213=CARTESIAN_POINT('Ctrl Pts',(0.0481015316490792,0.14670342243358,
0.750937880997459));
#15214=CARTESIAN_POINT('Ctrl Pts',(0.0966096924455767,0.120425158610167,
0.748291551118357));
#15215=CARTESIAN_POINT('Ctrl Pts',(0.122976945064223,0.0797827231418903,
0.745645221239255));
#15216=CARTESIAN_POINT('Ctrl Pts',(0.149344197682869,0.0391402876736125,
0.742998891360154));
#15217=CARTESIAN_POINT('Ctrl Pts',(0.153570542123663,-0.01586631943953,
0.740352561481052));
#15218=CARTESIAN_POINT('Ctrl Pts',(0.133721514043982,-0.0600597087159893,
0.73770623160195));
#15219=CARTESIAN_POINT('Ctrl Pts',(0.113872485964301,-0.104253097992448,
0.735059901722848));
#15220=CARTESIAN_POINT('Ctrl Pts',(0.0699480853641458,-0.137633269432224,
0.732413571843746));
#15221=CARTESIAN_POINT('Ctrl Pts',(0.0220532014503509,-0.144921593405036,
0.729767241964644));
#15222=CARTESIAN_POINT('Ctrl Pts',(-0.0258416824634434,-0.152209917377848,
0.727120912085542));
#15223=CARTESIAN_POINT('Ctrl Pts',(-0.0777070496908773,-0.133406393883698,
0.724474582206441));
#15224=CARTESIAN_POINT('Ctrl Pts',(-0.109803305666473,-0.0971176914572187,
0.721828252327339));
#15225=CARTESIAN_POINT('Ctrl Pts',(-0.133101311474982,-0.0707764758164216,
0.71990733641299));
#15226=CARTESIAN_POINT('Ctrl Pts',(-0.14598295937539,-0.0352223077304616,
0.71798642049864));
#15227=CARTESIAN_POINT('Ctrl Pts',(-0.146290249280603,0.000131112932912382,
0.716065504584291));
#15228=CARTESIAN_POINT('Ctrl Pts',(-0.146307221518699,0.000133045872591754,
0.708934495415711));
#15229=CARTESIAN_POINT('Ctrl Pts',(-0.145987367488279,-0.0358102803178394,
0.710888040627207));
#15230=CARTESIAN_POINT('Ctrl Pts',(-0.132622002370819,-0.0719663061161047,
0.712841585838703));
#15231=CARTESIAN_POINT('Ctrl Pts',(-0.1086007072861,-0.0984612847532928,
0.7147951310502));
#15232=CARTESIAN_POINT('Ctrl Pts',(-0.0760477256663158,-0.134366532557423,
0.71744252042446));
#15233=CARTESIAN_POINT('Ctrl Pts',(-0.0239252288417074,-0.152529358077047,
0.720089909798719));
#15234=CARTESIAN_POINT('Ctrl Pts',(0.0238920022682765,-0.144630254255197,
0.722737299172979));
#15235=CARTESIAN_POINT('Ctrl Pts',(0.071709233378259,-0.136731150433346,
0.725384688547239));
#15236=CARTESIAN_POINT('Ctrl Pts',(0.115221198773618,-0.102770117270024,
0.7280320779215));
#15237=CARTESIAN_POINT('Ctrl Pts',(0.134497183226257,-0.058303052428779,
0.730679467295759));
#15238=CARTESIAN_POINT('Ctrl Pts',(0.153773167678896,-0.0138359875875333,
0.733326856670019));
#15239=CARTESIAN_POINT('Ctrl Pts',(0.148813171188813,0.0411371089316358,
0.735974246044279));
#15240=CARTESIAN_POINT('Ctrl Pts',(0.121889126928366,0.0814357351225549,
0.738621635418539));
#15241=CARTESIAN_POINT('Ctrl Pts',(0.0949650826679194,0.121734361313473,
0.741269024792799));
#15242=CARTESIAN_POINT('Ctrl Pts',(0.0460769906371109,0.147358517176143,
0.74391641416706));
#15243=CARTESIAN_POINT('Ctrl Pts',(-0.00238189178169058,0.146571023090686,
0.74656380354132));
#15244=CARTESIAN_POINT('Ctrl Pts',(-0.0508407742004934,0.14578352900523,
0.74921119291558));
#15245=CARTESIAN_POINT('Ctrl Pts',(-0.0988704470072894,0.118584384971644,
0.751858582289839));
#15246=CARTESIAN_POINT('Ctrl Pts',(-0.124470852918682,0.0774321960944291,
0.754505971664099));
#15247=CARTESIAN_POINT('Ctrl Pts',(-0.138745545153454,0.0544858868428234,
0.75598214624797));
#15248=CARTESIAN_POINT('Ctrl Pts',(-0.146046671909043,0.027201385339783,
0.757458320831841));
#15249=CARTESIAN_POINT('Ctrl Pts',(-0.14612241379348,-4.54149644099216E-5,
0.758934495415711));
#15250=CARTESIAN_POINT('Origin',(0.,0.,0.));
#15251=CARTESIAN_POINT('',(-0.146495788566881,-0.000101744904923998,0.816065504584291));
#15252=CARTESIAN_POINT('',(-0.146473871348434,-0.000110945968026819,0.808934495415711));
#15253=CARTESIAN_POINT('',(-0.14635,-1.79227059055215E-17,0.));
#15254=CARTESIAN_POINT('Ctrl Pts',(-0.146495788566881,-0.000101744904923998,
0.816065504584291));
#15255=CARTESIAN_POINT('Ctrl Pts',(-0.14616118452328,0.0421270051992108,
0.813762715835428));
#15256=CARTESIAN_POINT('Ctrl Pts',(-0.126905337350145,0.0846218946815527,
0.811459927086565));
#15257=CARTESIAN_POINT('Ctrl Pts',(-0.0947343415465314,0.111866064832055,
0.809157138337701));
#15258=CARTESIAN_POINT('Ctrl Pts',(-0.0577639214515077,0.143174651664521,
0.806510808458599));
#15259=CARTESIAN_POINT('Ctrl Pts',(-0.00373742343573488,0.154342745753647,
0.803864478579497));
#15260=CARTESIAN_POINT('Ctrl Pts',(0.0426163743729279,0.140258534729872,
0.801218148700395));
#15261=CARTESIAN_POINT('Ctrl Pts',(0.0889701721815907,0.126174323706097,
0.798571818821294));
#15262=CARTESIAN_POINT('Ctrl Pts',(0.127651269783143,0.0868378075694234,
0.795925488942192));
#15263=CARTESIAN_POINT('Ctrl Pts',(0.140954720244851,0.040253928627653,
0.79327915906309));
#15264=CARTESIAN_POINT('Ctrl Pts',(0.154258170706558,-0.00632995031411615,
0.790632829183988));
#15265=CARTESIAN_POINT('Ctrl Pts',(0.14218397402842,-0.060161192060982,
0.787986499304886));
#15266=CARTESIAN_POINT('Ctrl Pts',(0.110258679990485,-0.0966003903512828,
0.785340169425784));
#15267=CARTESIAN_POINT('Ctrl Pts',(0.0783333859525485,-0.133039588641585,
0.782693839546682));
#15268=CARTESIAN_POINT('Ctrl Pts',(0.0265569945548152,-0.152086743475322,
0.780047509667581));
#15269=CARTESIAN_POINT('Ctrl Pts',(-0.021371625274328,-0.14502367242074,
0.777401179788479));
#15270=CARTESIAN_POINT('Ctrl Pts',(-0.0693002451034712,-0.137960601366157,
0.774754849909377));
#15271=CARTESIAN_POINT('Ctrl Pts',(-0.113381093364023,-0.104787304423254,
0.772108520030274));
#15272=CARTESIAN_POINT('Ctrl Pts',(-0.133437672293631,-0.0606877215103841,
0.769462190151172));
#15273=CARTESIAN_POINT('Ctrl Pts',(-0.1420188514214,-0.0418197768941368,
0.768329961628878));
#15274=CARTESIAN_POINT('Ctrl Pts',(-0.146202281842484,-0.0209517273285418,
0.767197733106584));
#15275=CARTESIAN_POINT('Ctrl Pts',(-0.1461301977291,-5.61458017395017E-5,
0.766065504584291));
#15276=CARTESIAN_POINT('Ctrl Pts',(-0.14612241379348,-4.54149644099216E-5,
0.758934495415711));
#15277=CARTESIAN_POINT('Ctrl Pts',(-0.146182508321779,-0.0216633562673834,
0.760105710206101));
#15278=CARTESIAN_POINT('Ctrl Pts',(-0.141694203021096,-0.0432575645610501,
0.76127692499649));
#15279=CARTESIAN_POINT('Ctrl Pts',(-0.132531725405586,-0.0626424774360703,
0.76244813978688));
#15280=CARTESIAN_POINT('Ctrl Pts',(-0.111821052965107,-0.106459728368519,
0.76509552916114));
#15281=CARTESIAN_POINT('Ctrl Pts',(-0.067228569068158,-0.138988996512573,
0.767742918535399));
#15282=CARTESIAN_POINT('Ctrl Pts',(-0.0191799219195066,-0.145330206128911,
0.770390307909659));
#15283=CARTESIAN_POINT('Ctrl Pts',(0.0288687252291434,-0.151671415745249,
0.773037697283919));
#15284=CARTESIAN_POINT('Ctrl Pts',(0.080373535629496,-0.131824566833873,
0.77568508665818));
#15285=CARTESIAN_POINT('Ctrl Pts',(0.111742660473083,-0.0948805356683208,
0.77833247603244));
#15286=CARTESIAN_POINT('Ctrl Pts',(0.14311178531667,-0.0579365045027684,
0.7809798654067));
#15287=CARTESIAN_POINT('Ctrl Pts',(0.154345224603492,-0.00389529108304171,
0.783627254780959));
#15288=CARTESIAN_POINT('Ctrl Pts',(0.140297486112651,0.0424894529122293,
0.786274644155219));
#15289=CARTESIAN_POINT('Ctrl Pts',(0.126249747621811,0.0888741969075009,
0.788922033529479));
#15290=CARTESIAN_POINT('Ctrl Pts',(0.0869208313533056,0.127602471478316,
0.79156942290374));
#15291=CARTESIAN_POINT('Ctrl Pts',(0.0403254011646538,0.140934737517831,
0.794216812278));
#15292=CARTESIAN_POINT('Ctrl Pts',(-0.00627002902399674,0.154267003557346,
0.79686420165226));
#15293=CARTESIAN_POINT('Ctrl Pts',(-0.0601319731327944,0.142203261065564,
0.799511591026519));
#15294=CARTESIAN_POINT('Ctrl Pts',(-0.0965888940360299,0.110269323781398,
0.802158980400779));
#15295=CARTESIAN_POINT('Ctrl Pts',(-0.127690529151203,0.0830262752573849,
0.804417485405756));
#15296=CARTESIAN_POINT('Ctrl Pts',(-0.146124951115714,0.0413218847513699,
0.806675990410734));
#15297=CARTESIAN_POINT('Ctrl Pts',(-0.146473871348434,-0.000110945968026819,
0.808934495415711));
#15298=CARTESIAN_POINT('Origin',(0.,0.,0.));
#15299=CARTESIAN_POINT('',(-0.146444331750498,0.000119944961782359,0.866065504584291));
#15300=CARTESIAN_POINT('',(-0.146471560192382,0.00011177640072981,0.858934495415711));
#15301=CARTESIAN_POINT('',(-0.14635,-1.79227059055215E-17,0.));
#15302=CARTESIAN_POINT('Ctrl Pts',(-0.146444331750498,0.000119944961782359,
0.866065504584291));
#15303=CARTESIAN_POINT('Ctrl Pts',(-0.146516681599632,0.00829054204730037,
0.865620358322474));
#15304=CARTESIAN_POINT('Ctrl Pts',(-0.145891801779796,0.0164500693154795,
0.865175212060658));
#15305=CARTESIAN_POINT('Ctrl Pts',(-0.14453063157077,0.0244848619971339,
0.864730065798841));
#15306=CARTESIAN_POINT('Ctrl Pts',(-0.136438672357208,0.0722505376181754,
0.862083735919739));
#15307=CARTESIAN_POINT('Ctrl Pts',(-0.102325254887189,0.115607931012472,
0.859437406040638));
#15308=CARTESIAN_POINT('Ctrl Pts',(-0.0578046270350215,0.134711681091902,
0.856791076161536));
#15309=CARTESIAN_POINT('Ctrl Pts',(-0.0132839991828526,0.153815431171333,
0.854144746282434));
#15310=CARTESIAN_POINT('Ctrl Pts',(0.0416438390514653,0.148665537935894,
0.851498416403331));
#15311=CARTESIAN_POINT('Ctrl Pts',(0.081837551941475,0.121619188541491,
0.848852086524229));
#15312=CARTESIAN_POINT('Ctrl Pts',(0.122031264831484,0.0945728391470885,
0.846205756645128));
#15313=CARTESIAN_POINT('Ctrl Pts',(0.147490852377186,0.0456300335937214,
0.843559426766026));
#15314=CARTESIAN_POINT('Ctrl Pts',(0.146563060809277,-0.0028073360113171,
0.840913096886925));
#15315=CARTESIAN_POINT('Ctrl Pts',(0.145635269241369,-0.0512447056163556,
0.838266767007823));
#15316=CARTESIAN_POINT('Ctrl Pts',(0.118320098559852,-0.0991766392730661,
0.835620437128721));
#15317=CARTESIAN_POINT('Ctrl Pts',(0.0771201321287374,-0.124663936845065,
0.832974107249619));
#15318=CARTESIAN_POINT('Ctrl Pts',(0.035920165697623,-0.150151234417064,
0.830327777370517));
#15319=CARTESIAN_POINT('Ctrl Pts',(-0.0191645964830881,-0.153193895904352,
0.827681447491415));
#15320=CARTESIAN_POINT('Ctrl Pts',(-0.0629209921278279,-0.132399247274726,
0.825035117612313));
#15321=CARTESIAN_POINT('Ctrl Pts',(-0.106677387772568,-0.111604598645101,
0.822388787733211));
#15322=CARTESIAN_POINT('Ctrl Pts',(-0.139105416881337,-0.0669726398985626,
0.819742457854109));
#15323=CARTESIAN_POINT('Ctrl Pts',(-0.145362260348583,-0.0189321207373897,
0.817096127975007));
#15324=CARTESIAN_POINT('Ctrl Pts',(-0.146174510965348,-0.0126955988357878,
0.816752586844768));
#15325=CARTESIAN_POINT('Ctrl Pts',(-0.146545706411658,-0.00640163348415362,
0.81640904571453));
#15326=CARTESIAN_POINT('Ctrl Pts',(-0.146495788566881,-0.000101744904923998,
0.816065504584291));
#15327=CARTESIAN_POINT('Ctrl Pts',(-0.146473871348434,-0.000110945968026819,
0.808934495415711));
#15328=CARTESIAN_POINT('Ctrl Pts',(-0.146533950748007,-0.00724512552769256,
0.809323379784994));
#15329=CARTESIAN_POINT('Ctrl Pts',(-0.146057826922151,-0.0143712538186879,
0.809712264154277));
#15330=CARTESIAN_POINT('Ctrl Pts',(-0.145017839345608,-0.0214141189368497,
0.81010114852356));
#15331=CARTESIAN_POINT('Ctrl Pts',(-0.137937966054276,-0.0693594922943736,
0.81274853789782));
#15332=CARTESIAN_POINT('Ctrl Pts',(-0.104726321773939,-0.113446106932874,
0.81539592727208));
#15333=CARTESIAN_POINT('Ctrl Pts',(-0.0605955455659204,-0.133480028752914,
0.818043316646339));
#15334=CARTESIAN_POINT('Ctrl Pts',(-0.0164647693578984,-0.153513950572954,
0.820690706020599));
#15335=CARTESIAN_POINT('Ctrl Pts',(0.0385851387778066,-0.149495179574532,
0.823338095394859));
#15336=CARTESIAN_POINT('Ctrl Pts',(0.0793384931690736,-0.12326451930694,
0.825985484769119));
#15337=CARTESIAN_POINT('Ctrl Pts',(0.120091847560339,-0.0970338590393495,
0.828632874143379));
#15338=CARTESIAN_POINT('Ctrl Pts',(0.146548648207165,-0.0485913095025905,
0.83128026351764));
#15339=CARTESIAN_POINT('Ctrl Pts',(0.146590321408106,-0.000126046730599388,
0.833927652891899));
#15340=CARTESIAN_POINT('Ctrl Pts',(0.146631994609047,0.0483392160413931,
0.836575042266159));
#15341=CARTESIAN_POINT('Ctrl Pts',(0.120258540364101,0.0968271920486179,
0.839222431640419));
#15342=CARTESIAN_POINT('Ctrl Pts',(0.0795503554414038,0.123127897600245,
0.841869821014679));
#15343=CARTESIAN_POINT('Ctrl Pts',(0.0388421705187073,0.149428603151872,
0.844517210388939));
#15344=CARTESIAN_POINT('Ctrl Pts',(-0.0162007450817403,0.153542038247903,
0.8471645997632));
#15345=CARTESIAN_POINT('Ctrl Pts',(-0.0603659086281491,0.133584038319734,
0.84981198913746));
#15346=CARTESIAN_POINT('Ctrl Pts',(-0.104531072174558,0.113626038391565,
0.85245937851172));
#15347=CARTESIAN_POINT('Ctrl Pts',(-0.137818483666928,0.0695966034391962,
0.855106767885979));
#15348=CARTESIAN_POINT('Ctrl Pts',(-0.144980798768897,0.0216634763286692,
0.857754157260239));
#15349=CARTESIAN_POINT('Ctrl Pts',(-0.146045237806912,0.0145398171508471,
0.858147603312063));
#15350=CARTESIAN_POINT('Ctrl Pts',(-0.146532654486068,0.00732993751956911,
0.858541049363887));
#15351=CARTESIAN_POINT('Ctrl Pts',(-0.146471560192382,0.00011177640072981,
0.858934495415711));
#15352=CARTESIAN_POINT('Origin',(0.,0.,0.));
#15353=CARTESIAN_POINT('',(-0.146114231148477,2.69008449349656E-5,0.916065504584291));
#15354=CARTESIAN_POINT('',(-0.146121644853617,4.41067432152685E-5,0.908934495415711));
#15355=CARTESIAN_POINT('',(-0.14635,-1.79227059055215E-17,0.));
#15356=CARTESIAN_POINT('Ctrl Pts',(-0.146114231148477,2.69008449349656E-5,
0.916065504584291));
#15357=CARTESIAN_POINT('Ctrl Pts',(-0.146151635159142,0.0228038459942234,
0.914831670930419));
#15358=CARTESIAN_POINT('Ctrl Pts',(-0.141147538069067,0.0455652341090756,
0.913597837276548));
#15359=CARTESIAN_POINT('Ctrl Pts',(-0.131015765267123,0.0657531838068269,
0.912364003622676));
#15360=CARTESIAN_POINT('Ctrl Pts',(-0.109285110563454,0.109052354902802,
0.909717673743574));
#15361=CARTESIAN_POINT('Ctrl Pts',(-0.0639662294071284,0.140513248471977,
0.907071343864472));
#15362=CARTESIAN_POINT('Ctrl Pts',(-0.015802286694576,0.145735718560985,
0.90442501398537));
#15363=CARTESIAN_POINT('Ctrl Pts',(0.0323616560179757,0.150958188649994,
0.901778684106268));
#15364=CARTESIAN_POINT('Ctrl Pts',(0.0833706602867547,0.129942235258839,
0.899132354227166));
#15365=CARTESIAN_POINT('Ctrl Pts',(0.113877102345416,0.0923071908936453,
0.896486024348064));
#15366=CARTESIAN_POINT('Ctrl Pts',(0.144383544404078,0.0546721465284523,
0.893839694468962));
#15367=CARTESIAN_POINT('Ctrl Pts',(0.15438742425262,0.000418011189221586,
0.891193364589861));
#15368=CARTESIAN_POINT('Ctrl Pts',(0.139309808695705,-0.0456222438118789,
0.888547034710759));
#15369=CARTESIAN_POINT('Ctrl Pts',(0.124232193138789,-0.0916624988129813,
0.885900704831657));
#15370=CARTESIAN_POINT('Ctrl Pts',(0.0840730821764119,-0.129488873475953,
0.883254374952555));
#15371=CARTESIAN_POINT('Ctrl Pts',(0.0372139327097935,-0.141787641004198,
0.880608045073453));
#15372=CARTESIAN_POINT('Ctrl Pts',(-0.00964521675682358,-0.154086408532443,
0.877961715194351));
#15373=CARTESIAN_POINT('Ctrl Pts',(-0.0632044047276821,-0.140857568925962,
0.875315385315249));
#15374=CARTESIAN_POINT('Ctrl Pts',(-0.0989487482345592,-0.108156170198829,
0.872669055436147));
#15375=CARTESIAN_POINT('Ctrl Pts',(-0.128680439645858,-0.0809555616469925,
0.870467871818862));
#15376=CARTESIAN_POINT('Ctrl Pts',(-0.146086572253705,-0.0402824710322022,
0.868266688201576));
#15377=CARTESIAN_POINT('Ctrl Pts',(-0.146444331750498,0.000119944961782359,
0.866065504584291));
#15378=CARTESIAN_POINT('Ctrl Pts',(-0.146471560192382,0.00011177640072981,
0.858934495415711));
#15379=CARTESIAN_POINT('Ctrl Pts',(-0.146121567926216,-0.0412390669452651,
0.861188438738147));
#15380=CARTESIAN_POINT('Ctrl Pts',(-0.127770397964496,-0.0828616943330661,
0.863442382060584));
#15381=CARTESIAN_POINT('Ctrl Pts',(-0.096778382793969,-0.110103055552942,
0.86569632538302));
#15382=CARTESIAN_POINT('Ctrl Pts',(-0.0603764330055066,-0.142099641055337,
0.86834371475728));
#15383=CARTESIAN_POINT('Ctrl Pts',(-0.00653531471701479,-0.154255992791443,
0.870991104131539));
#15384=CARTESIAN_POINT('Ctrl Pts',(0.040082974241256,-0.14100387723139,
0.873638493505799));
#15385=CARTESIAN_POINT('Ctrl Pts',(0.0867012631995282,-0.127751761671338,
0.876285882880059));
#15386=CARTESIAN_POINT('Ctrl Pts',(0.12609672282758,-0.0890911788151255,
0.878933272254319));
#15387=CARTESIAN_POINT('Ctrl Pts',(0.140224208991091,-0.042730661487191,
0.88158066162858));
#15388=CARTESIAN_POINT('Ctrl Pts',(0.154351695154603,0.00362985584074295,
0.88422805100284));
#15389=CARTESIAN_POINT('Ctrl Pts',(0.143211207853577,0.057690307640398,
0.886875440377099));
#15390=CARTESIAN_POINT('Ctrl Pts',(0.111905662524754,0.09468823006692,0.889522829751359));
#15391=CARTESIAN_POINT('Ctrl Pts',(0.0806001171959318,0.131686152493442,
0.892170219125619));
#15392=CARTESIAN_POINT('Ctrl Pts',(0.0291295138393125,0.15162154554683,
0.894817608499879));
#15393=CARTESIAN_POINT('Ctrl Pts',(-0.0189299673197759,0.145362975188259,
0.897464997874139));
#15394=CARTESIAN_POINT('Ctrl Pts',(-0.0669894484788628,0.139104404829688,
0.9001123872484));
#15395=CARTESIAN_POINT('Ctrl Pts',(-0.11163780744042,0.10665187105916,0.902759776622659));
#15396=CARTESIAN_POINT('Ctrl Pts',(-0.132423802349956,0.0628703013313112,
0.905407165996919));
#15397=CARTESIAN_POINT('Ctrl Pts',(-0.141655418982822,0.043425734493323,
0.90658294246985));
#15398=CARTESIAN_POINT('Ctrl Pts',(-0.146180218154578,0.0217465313827003,
0.907758718942781));
#15399=CARTESIAN_POINT('Ctrl Pts',(-0.146121644853617,4.41067432152685E-5,
0.908934495415711));
#15400=CARTESIAN_POINT('Origin',(0.,0.,0.));
#15401=CARTESIAN_POINT('',(-0.146345621585321,-0.000133809880645736,0.966065504584291));
#15402=CARTESIAN_POINT('',(-0.146309694201085,-0.000133223314395004,0.958934495415711));
#15403=CARTESIAN_POINT('',(-0.14635,-1.79227059055215E-17,0.));
#15404=CARTESIAN_POINT('Ctrl Pts',(-0.146345621585321,-0.000133809880645736,
0.966065504584291));
#15405=CARTESIAN_POINT('Ctrl Pts',(-0.146004672532387,0.0370537288701324,
0.964042983538364));
#15406=CARTESIAN_POINT('Ctrl Pts',(-0.131578083002406,0.0744765756810296,
0.962020462492437));
#15407=CARTESIAN_POINT('Ctrl Pts',(-0.106003654037246,0.101251356830495,
0.959997941446511));
#15408=CARTESIAN_POINT('Ctrl Pts',(-0.0725412702228666,0.136284319036219,
0.957351611567409));
#15409=CARTESIAN_POINT('Ctrl Pts',(-0.0199938687303381,0.153087872523943,
0.954705281688306));
#15410=CARTESIAN_POINT('Ctrl Pts',(0.0275867780614433,0.143970766496025,
0.952058951809204));
#15411=CARTESIAN_POINT('Ctrl Pts',(0.0751674248532248,0.134853660468108,
0.949412621930102));
#15412=CARTESIAN_POINT('Ctrl Pts',(0.11778131694426,0.0998158949245492,
0.946766292051));
#15413=CARTESIAN_POINT('Ctrl Pts',(0.135923405490256,0.0548948063954655,
0.944119962171899));
#15414=CARTESIAN_POINT('Ctrl Pts',(0.154065494036253,0.0099737178663825,
0.941473632292797));
#15415=CARTESIAN_POINT('Ctrl Pts',(0.147735779037212,-0.0448306936482241,
0.938827302413695));
#15416=CARTESIAN_POINT('Ctrl Pts',(0.119831470632095,-0.0844335867733556,
0.936180972534593));
#15417=CARTESIAN_POINT('Ctrl Pts',(0.0919271622269763,-0.124036479898489,
0.933534642655491));
#15418=CARTESIAN_POINT('Ctrl Pts',(0.0424482604157787,-0.148437854634144,
0.93088831277639));
#15419=CARTESIAN_POINT('Ctrl Pts',(-0.00595796300272124,-0.146468817862788,
0.928241982897288));
#15420=CARTESIAN_POINT('Ctrl Pts',(-0.0543641864212212,-0.144499781091432,
0.925595653018186));
#15421=CARTESIAN_POINT('Ctrl Pts',(-0.101697731447024,-0.116160332813065,
0.922949323139084));
#15422=CARTESIAN_POINT('Ctrl Pts',(-0.126293289834417,-0.0744218843624929,
0.920302993259982));
#15423=CARTESIAN_POINT('Ctrl Pts',(-0.139421333187579,-0.052143709087005,
0.918890497034752));
#15424=CARTESIAN_POINT('Ctrl Pts',(-0.146071410932229,-0.0260482098028304,
0.917478000809521));
#15425=CARTESIAN_POINT('Ctrl Pts',(-0.146114231148477,2.69008449349656E-5,
0.916065504584291));
#15426=CARTESIAN_POINT('Ctrl Pts',(-0.146121644853617,4.41067432152685E-5,
0.908934495415711));
#15427=CARTESIAN_POINT('Ctrl Pts',(-0.146048333958771,-0.027118852224649,
0.910406108317041));
#15428=CARTESIAN_POINT('Ctrl Pts',(-0.138795050353101,-0.0543181883240968,
0.91187772121837));
#15429=CARTESIAN_POINT('Ctrl Pts',(-0.124603830013468,-0.0772180274565794,
0.9133493341197));
#15430=CARTESIAN_POINT('Ctrl Pts',(-0.0990742319099257,-0.118414180831446,
0.91599672349396));
#15431=CARTESIAN_POINT('Ctrl Pts',(-0.0510914048453256,-0.145695881896007,
0.91864411286822));
#15432=CARTESIAN_POINT('Ctrl Pts',(-0.00263394834681351,-0.146566710184873,
0.92129150224248));
#15433=CARTESIAN_POINT('Ctrl Pts',(0.0458235081516972,-0.147437538473739,
0.92393889161674));
#15434=CARTESIAN_POINT('Ctrl Pts',(0.0947555940841207,-0.121897493986912,
0.926586280990999));
#15435=CARTESIAN_POINT('Ctrl Pts',(0.121748900601314,-0.0816452290135895,
0.929233670365259));
#15436=CARTESIAN_POINT('Ctrl Pts',(0.148742207118509,-0.0413929640402651,
0.931881059739519));
#15437=CARTESIAN_POINT('Ctrl Pts',(0.153796734220472,0.0135715214195569,
0.93452844911378));
#15438=CARTESIAN_POINT('Ctrl Pts',(0.134597248858856,0.0580716696672091,
0.93717583848804));
#15439=CARTESIAN_POINT('Ctrl Pts',(0.115397763497239,0.102571817914861,
0.9398232278623));
#15440=CARTESIAN_POINT('Ctrl Pts',(0.0719442656720451,0.136607628950342,
0.942470617236559));
#15441=CARTESIAN_POINT('Ctrl Pts',(0.0241406894609324,0.144588953003544,
0.945118006610819));
#15442=CARTESIAN_POINT('Ctrl Pts',(-0.023662886750181,0.152570277056746,
0.947765395985079));
#15443=CARTESIAN_POINT('Ctrl Pts',(-0.0758165413472122,0.134497114127667,
0.950412785359339));
#15444=CARTESIAN_POINT('Ctrl Pts',(-0.108431221550465,0.0986479012011113,
0.953060174733599));
#15445=CARTESIAN_POINT('Ctrl Pts',(-0.132554242808212,0.0721325001574252,
0.955018281627637));
#15446=CARTESIAN_POINT('Ctrl Pts',(-0.145988218858404,0.0358924841874147,
0.956976388521674));
#15447=CARTESIAN_POINT('Ctrl Pts',(-0.146309694201085,-0.000133223314395004,
0.958934495415711));
#15448=CARTESIAN_POINT('Origin',(0.,0.,0.));
#15449=CARTESIAN_POINT('',(-0.146565171121453,5.44893591410845E-5,1.01606550458429));
#15450=CARTESIAN_POINT('',(-0.146582076026177,3.15354312248815E-5,1.00893449541571));
#15451=CARTESIAN_POINT('',(-0.14635,-1.79227059055215E-17,0.));
#15452=CARTESIAN_POINT('Ctrl Pts',(-0.146565171121453,5.44893591410845E-5,
1.01606550458429));
#15453=CARTESIAN_POINT('Ctrl Pts',(-0.146579596851449,0.00307427920823236,
1.01590062602541));
#15454=CARTESIAN_POINT('Ctrl Pts',(-0.146494352296349,0.00609323927190738,
1.01573574746653));
#15455=CARTESIAN_POINT('Ctrl Pts',(-0.146306854564556,0.00910583530985269,
1.01557086890765));
#15456=CARTESIAN_POINT('Ctrl Pts',(-0.143297482980539,0.0574585317612167,
1.01292453902855));
#15457=CARTESIAN_POINT('Ctrl Pts',(-0.11394685994478,0.104171803331984,
1.01027820914945));
#15458=CARTESIAN_POINT('Ctrl Pts',(-0.0716892273871119,0.127864250695428,
1.00763187927034));
#15459=CARTESIAN_POINT('Ctrl Pts',(-0.0294315948294418,0.151556698058874,
1.00498554939124));
#15460=CARTESIAN_POINT('Ctrl Pts',(0.0257330472501378,0.152228321214993,
1.00233921951214));
#15461=CARTESIAN_POINT('Ctrl Pts',(0.0685549742796134,0.129571707678744,
0.999692889633039));
#15462=CARTESIAN_POINT('Ctrl Pts',(0.111376901309088,0.106915094142495,
0.997046559753937));
#15463=CARTESIAN_POINT('Ctrl Pts',(0.141856113288459,0.0609302439138786,
0.994400229874835));
#15464=CARTESIAN_POINT('Ctrl Pts',(0.146041795372579,0.0126651464112397,
0.991753899995733));
#15465=CARTESIAN_POINT('Ctrl Pts',(0.150227477456699,-0.0355999510913994,
0.989107570116631));
#15466=CARTESIAN_POINT('Ctrl Pts',(0.128119629645567,-0.0861452958680607,
0.986461240237529));
#15467=CARTESIAN_POINT('Ctrl Pts',(0.0898373616998479,-0.115835488396583,
0.983814910358427));
#15468=CARTESIAN_POINT('Ctrl Pts',(0.051555093754129,-0.145525680925106,
0.981168580479325));
#15469=CARTESIAN_POINT('Ctrl Pts',(-0.00290159432617693,-0.154360721205491,
0.978522250600224));
#15470=CARTESIAN_POINT('Ctrl Pts',(-0.0486070196525971,-0.138296672301818,
0.975875920721122));
#15471=CARTESIAN_POINT('Ctrl Pts',(-0.0943124449790173,-0.122232623398145,
0.97322959084202));
#15472=CARTESIAN_POINT('Ctrl Pts',(-0.131266607551552,-0.081269485310415,
0.970583260962917));
#15473=CARTESIAN_POINT('Ctrl Pts',(-0.142555005769704,-0.0341567308046872,
0.967936931083816));
#15474=CARTESIAN_POINT('Ctrl Pts',(-0.145215975052668,-0.0230510282813687,
0.967313122250641));
#15475=CARTESIAN_POINT('Ctrl Pts',(-0.146450780951306,-0.0116036114945705,
0.966689313417466));
#15476=CARTESIAN_POINT('Ctrl Pts',(-0.146345621585321,-0.000133809880645736,
0.966065504584291));
#15477=CARTESIAN_POINT('Ctrl Pts',(-0.146309694201085,-0.000133223314395004,
0.958934495415711));
#15478=CARTESIAN_POINT('Ctrl Pts',(-0.146422858258782,-0.0128148032088542,
0.959623777895933));
#15479=CARTESIAN_POINT('Ctrl Pts',(-0.14491119500038,-0.0254698272036438,
0.960313060376156));
#15480=CARTESIAN_POINT('Ctrl Pts',(-0.141668994059001,-0.037664762585484,
0.961002342856379));
#15481=CARTESIAN_POINT('Ctrl Pts',(-0.129216380554811,-0.0845029505214961,
0.963649732230639));
#15482=CARTESIAN_POINT('Ctrl Pts',(-0.0912354477369537,-0.12455406346949,
0.966297121604899));
#15483=CARTESIAN_POINT('Ctrl Pts',(-0.0451234138007503,-0.1394726343957,
0.968944510979159));
#15484=CARTESIAN_POINT('Ctrl Pts',(0.00098862013545236,-0.154391205321909,
0.97159190035342));
#15485=CARTESIAN_POINT('Ctrl Pts',(0.055231755190001,-0.144177234226336,
0.974239289727679));
#15486=CARTESIAN_POINT('Ctrl Pts',(0.0927598492034174,-0.113509244531313,
0.976886679101939));
#15487=CARTESIAN_POINT('Ctrl Pts',(0.130287943216833,-0.0828412548362905,
0.979534068476199));
#15488=CARTESIAN_POINT('Ctrl Pts',(0.151100996189117,-0.0317192465418168,
0.982181457850459));
#15489=CARTESIAN_POINT('Ctrl Pts',(0.145665560755875,0.0164402745715088,
0.984828847224719));
#15490=CARTESIAN_POINT('Ctrl Pts',(0.140230125322634,0.0645997956848379,
0.987476236598979));
#15491=CARTESIAN_POINT('Ctrl Pts',(0.108546201483865,0.109796829617019,
0.990123625973239));
#15492=CARTESIAN_POINT('Ctrl Pts',(0.0651266538643092,0.131328813193254,
0.992771015347499));
#15493=CARTESIAN_POINT('Ctrl Pts',(0.0217071062447581,0.152860796769488,
0.995418404721759));
#15494=CARTESIAN_POINT('Ctrl Pts',(-0.0334480651555777,0.15072772998978,
0.998065794096019));
#15495=CARTESIAN_POINT('Ctrl Pts',(-0.0750749586823209,0.125906667008376,
1.00071318347028));
#15496=CARTESIAN_POINT('Ctrl Pts',(-0.116701852209067,0.101085604026969,
1.00336057284454));
#15497=CARTESIAN_POINT('Ctrl Pts',(-0.144800467862219,0.053576544843864,
1.0060079622188));
#15498=CARTESIAN_POINT('Ctrl Pts',(-0.146500196332402,0.00514107896046776,
1.00865535159306));
#15499=CARTESIAN_POINT('Ctrl Pts',(-0.146559936783033,0.00343871495990628,
1.00874839953394));
#15500=CARTESIAN_POINT('Ctrl Pts',(-0.146587066279139,0.00173520655478852,
1.00884144747483));
#15501=CARTESIAN_POINT('Ctrl Pts',(-0.146582076026177,3.15354312248815E-5,
1.00893449541571));
#15502=CARTESIAN_POINT('Origin',(0.,0.,0.));
#15503=CARTESIAN_POINT('',(-0.146184049129756,9.96948043307314E-5,1.06606550458429));
#15504=CARTESIAN_POINT('',(-0.146216477546812,0.000114345603752017,1.05893449541571));
#15505=CARTESIAN_POINT('',(-0.14635,-1.79227059055215E-17,0.));
#15506=CARTESIAN_POINT('Ctrl Pts',(-0.146184049129756,9.96948043307314E-5,
1.06606550458429));
#15507=CARTESIAN_POINT('Ctrl Pts',(-0.146294264763128,0.0176817746259609,
1.06511193863336));
#15508=CARTESIAN_POINT('Ctrl Pts',(-0.143360807533043,0.0352283113603788,
1.06415837268242));
#15509=CARTESIAN_POINT('Ctrl Pts',(-0.13721959397524,0.0515693218739058,
1.06320480673148));
#15510=CARTESIAN_POINT('Ctrl Pts',(-0.120176538991979,0.0969187854681546,
1.06055847685238));
#15511=CARTESIAN_POINT('Ctrl Pts',(-0.0784283132238915,0.132983650068601,
1.05791214697328));
#15512=CARTESIAN_POINT('Ctrl Pts',(-0.0310837364199337,0.143256459747686,
1.05526581709418));
#15513=CARTESIAN_POINT('Ctrl Pts',(0.0162608403840241,0.153529269426771,
1.05261948721508));
#15514=CARTESIAN_POINT('Ctrl Pts',(0.0692017682238519,0.138010024184496,
1.04997315733597));
#15515=CARTESIAN_POINT('Ctrl Pts',(0.103507151520239,0.103802126728842,
1.04732682745687));
#15516=CARTESIAN_POINT('Ctrl Pts',(0.137812534816628,0.0695942292731864,
1.04468049757777));
#15517=CARTESIAN_POINT('Ctrl Pts',(0.153482373569574,0.01669767960415,1.04203416769867));
#15518=CARTESIAN_POINT('Ctrl Pts',(0.143344336052008,-0.0306759392859165,
1.03938783781957));
#15519=CARTESIAN_POINT('Ctrl Pts',(0.133206298534443,-0.0780495581759789,
1.03674150794047));
#15520=CARTESIAN_POINT('Ctrl Pts',(0.0972603847463712,-0.119900246287072,
1.03409517806136));
#15521=CARTESIAN_POINT('Ctrl Pts',(0.0519596049571008,-0.137072285243832,
1.03144884818226));
#15522=CARTESIAN_POINT('Ctrl Pts',(0.00665882516783032,-0.154244324200591,
1.02880251830316));
#15523=CARTESIAN_POINT('Ctrl Pts',(-0.0479968206226384,-0.146737714003016,
1.02615618842406));
#15524=CARTESIAN_POINT('Ctrl Pts',(-0.0869905834517384,-0.11798834823825,
1.02350985854496));
#15525=CARTESIAN_POINT('Ctrl Pts',(-0.123554854979944,-0.0910302005802824,
1.02102840722473));
#15526=CARTESIAN_POINT('Ctrl Pts',(-0.146348061346918,-0.0453938791777224,
1.01854695590451));
#15527=CARTESIAN_POINT('Ctrl Pts',(-0.146565171121453,5.44893591410845E-5,
1.01606550458429));
#15528=CARTESIAN_POINT('Ctrl Pts',(-0.146582076026177,3.15354312248815E-5,
1.00893449541571));
#15529=CARTESIAN_POINT('Ctrl Pts',(-0.146445084172466,-0.0467374494427972,
1.01148883684909));
#15530=CARTESIAN_POINT('Ctrl Pts',(-0.122102455869861,-0.0936290599181376,
1.01404317828246));
#15531=CARTESIAN_POINT('Ctrl Pts',(-0.0837162036049941,-0.120334265578335,
1.01659751971584));
#15532=CARTESIAN_POINT('Ctrl Pts',(-0.0439316411201867,-0.14801227165006,
1.0192449090901));
#15533=CARTESIAN_POINT('Ctrl Pts',(0.0109383251366414,-0.154006411209824,
1.02189229846436));
#15534=CARTESIAN_POINT('Ctrl Pts',(0.0557604321169594,-0.135571060438576,
1.02453968783862));
#15535=CARTESIAN_POINT('Ctrl Pts',(0.100582539097277,-0.11713570966733,
1.02718707721288));
#15536=CARTESIAN_POINT('Ctrl Pts',(0.135356786801084,-0.0742708685650716,
1.02983446658714));
#15537=CARTESIAN_POINT('Ctrl Pts',(0.144154783532934,-0.0266108361928598,
1.0324818559614));
#15538=CARTESIAN_POINT('Ctrl Pts',(0.152952780264784,0.0210491961793507,
1.03512924533566));
#15539=CARTESIAN_POINT('Ctrl Pts',(0.135774526024679,0.0735044198215165,
1.03777663470992));
#15540=CARTESIAN_POINT('Ctrl Pts',(0.100488543649143,0.106727647840587,
1.04042402408418));
#15541=CARTESIAN_POINT('Ctrl Pts',(0.0652025612736062,0.139950875859659,
1.04307141345844));
#15542=CARTESIAN_POINT('Ctrl Pts',(0.0118088507626404,0.153942108255635,
1.0457188028327));
#15543=CARTESIAN_POINT('Ctrl Pts',(-0.0352355257975899,0.142292641904202,
1.04836619220696));
#15544=CARTESIAN_POINT('Ctrl Pts',(-0.0822799023578202,0.130643175552769,
1.05101358158122));
#15545=CARTESIAN_POINT('Ctrl Pts',(-0.122974944967313,0.0933530104539243,
1.05366097095548));
#15546=CARTESIAN_POINT('Ctrl Pts',(-0.138680233730631,0.0475029577050484,
1.05630836032974));
#15547=CARTESIAN_POINT('Ctrl Pts',(-0.143873300563147,0.0323423075707214,
1.05718373869173));
#15548=CARTESIAN_POINT('Ctrl Pts',(-0.146334133026589,0.0162457690968458,
1.05805911705372));
#15549=CARTESIAN_POINT('Ctrl Pts',(-0.146216477546812,0.000114345603752017,
1.05893449541571));
#15550=CARTESIAN_POINT('Origin',(0.,0.,0.));
#15551=CARTESIAN_POINT('',(-0.146204073634541,-0.000109175101205505,1.11606550458429));
#15552=CARTESIAN_POINT('',(-0.146170555016798,-9.22629125885076E-5,1.10893449541571));
#15553=CARTESIAN_POINT('',(-0.14635,-1.79227059055215E-17,0.));
#15554=CARTESIAN_POINT('Ctrl Pts',(-0.146204073634541,-0.000109175101205505,
1.11606550458429));
#15555=CARTESIAN_POINT('Ctrl Pts',(-0.145981599624502,0.032003853555373,
1.1143232512413));
#15556=CARTESIAN_POINT('Ctrl Pts',(-0.135565881201595,0.0642480963468658,
1.11258099789831));
#15557=CARTESIAN_POINT('Ctrl Pts',(-0.11609067353381,0.0895073597405865,
1.11083874455532));
#15558=CARTESIAN_POINT('Ctrl Pts',(-0.0865095427755784,0.127873963375947,
1.10819241467622));
#15559=CARTESIAN_POINT('Ctrl Pts',(-0.0360273159486943,0.150125560802435,
1.10554608479712));
#15560=CARTESIAN_POINT('Ctrl Pts',(0.0122494975033169,0.14607724579886,
1.10289975491801));
#15561=CARTESIAN_POINT('Ctrl Pts',(0.0605263109553308,0.142028930795284,
1.10025342503891));
#15562=CARTESIAN_POINT('Ctrl Pts',(0.10659771103247,0.111680703361642,1.09760709515981));
#15563=CARTESIAN_POINT('Ctrl Pts',(0.129376093089052,0.0689234246557527,
1.09496076528071));
#15564=CARTESIAN_POINT('Ctrl Pts',(0.152154475145634,0.0261661459498645,
1.09231443540161));
#15565=CARTESIAN_POINT('Ctrl Pts',(0.151639839181659,-0.0290001840282729,
1.0896681055225));
#15566=CARTESIAN_POINT('Ctrl Pts',(0.128067742174483,-0.0713250681289163,
1.0870217756434));
#15567=CARTESIAN_POINT('Ctrl Pts',(0.104495645167307,-0.11364995222956,
1.0843754457643));
#15568=CARTESIAN_POINT('Ctrl Pts',(0.0578660871169326,-0.143133390452712,
1.0817291158852));
#15569=CARTESIAN_POINT('Ctrl Pts',(0.00952215035475689,-0.146280349267719,
1.0790827860061));
#15570=CARTESIAN_POINT('Ctrl Pts',(-0.0388217864074202,-0.149427308082725,
1.07643645612699));
#15571=CARTESIAN_POINT('Ctrl Pts',(-0.0888801018813974,-0.126237787489585,
1.07379012624789));
#15572=CARTESIAN_POINT('Ctrl Pts',(-0.117740317519168,-0.0873259958989869,
1.07114379636879));
#15573=CARTESIAN_POINT('Ctrl Pts',(-0.136201180005177,-0.0624354946409797,
1.06945103244062));
#15574=CARTESIAN_POINT('Ctrl Pts',(-0.145988395071105,-0.0311118962502767,
1.06775826851246));
#15575=CARTESIAN_POINT('Ctrl Pts',(-0.146184049129756,9.96948043307314E-5,
1.06606550458429));
#15576=CARTESIAN_POINT('Ctrl Pts',(-0.146216477546812,0.000114345603752017,
1.05893449541571));
#15577=CARTESIAN_POINT('Ctrl Pts',(-0.145978309898544,-0.0325401742182177,
1.06070650642798));
#15578=CARTESIAN_POINT('Ctrl Pts',(-0.135174246449945,-0.06533764273189,
1.06247851744025));
#15579=CARTESIAN_POINT('Ctrl Pts',(-0.115079600404687,-0.0908043159161929,
1.06425052845252));
#15580=CARTESIAN_POINT('Ctrl Pts',(-0.0850581433982766,-0.128851596389654,
1.06689791782678));
#15581=CARTESIAN_POINT('Ctrl Pts',(-0.0342996944683099,-0.150536216937668,
1.06954530720104));
#15582=CARTESIAN_POINT('Ctrl Pts',(0.0139457694684962,-0.145925507476389,
1.0721926965753));
#15583=CARTESIAN_POINT('Ctrl Pts',(0.0621912334052997,-0.14131479801511,
1.07484008594956));
#15584=CARTESIAN_POINT('Ctrl Pts',(0.107923712348941,-0.110408758544542,
1.07748747532382));
#15585=CARTESIAN_POINT('Ctrl Pts',(0.1301953818052,-0.0673639426912374,
1.08013486469808));
#15586=CARTESIAN_POINT('Ctrl Pts',(0.15246705126146,-0.024319126837932,
1.08278225407234));
#15587=CARTESIAN_POINT('Ctrl Pts',(0.151277911230334,0.0308644653981125,
1.0854296434466));
#15588=CARTESIAN_POINT('Ctrl Pts',(0.127172648928576,0.0729099141598672,
1.08807703282086));
#15589=CARTESIAN_POINT('Ctrl Pts',(0.103067386626818,0.114955362921624,
1.09072442219512));
#15590=CARTESIAN_POINT('Ctrl Pts',(0.0560460020544268,0.143862668209093,
1.09337181156938));
#15591=CARTESIAN_POINT('Ctrl Pts',(0.00764670469074742,0.146390799320458,
1.09601920094364));
#15592=CARTESIAN_POINT('Ctrl Pts',(-0.0407525926729279,0.148918930431823,
1.0986665903179));
#15593=CARTESIAN_POINT('Ctrl Pts',(-0.0905298028278899,0.125067887367091,
1.10131397969216));
#15594=CARTESIAN_POINT('Ctrl Pts',(-0.11888440661962,0.0857626730052823,
1.10396136906642));
#15595=CARTESIAN_POINT('Ctrl Pts',(-0.136639133674055,0.0611510311732957,
1.10561907784952));
#15596=CARTESIAN_POINT('Ctrl Pts',(-0.145994366384503,0.0304800321277272,
1.10727678663261));
#15597=CARTESIAN_POINT('Ctrl Pts',(-0.146170555016798,-9.22629125885076E-5,
1.10893449541571));
#15598=CARTESIAN_POINT('Origin',(0.,0.,0.));
#15599=CARTESIAN_POINT('',(-0.146577386142569,-3.88073511912723E-5,1.16606550458429));
#15600=CARTESIAN_POINT('',(-0.146552328192774,-6.73160170860698E-5,1.15893449541571));
#15601=CARTESIAN_POINT('',(-0.14635,-1.79227059055215E-17,0.));
#15602=CARTESIAN_POINT('Ctrl Pts',(-0.146577386142569,-3.88073511912723E-5,
1.16606550458429));
#15603=CARTESIAN_POINT('Ctrl Pts',(-0.146413350709018,0.0463056768050285,
1.16353456384924));
#15604=CARTESIAN_POINT('Ctrl Pts',(-0.122574225104448,0.0927954474992645,
1.1610036231142));
#15605=CARTESIAN_POINT('Ctrl Pts',(-0.0847742546295189,0.119590709008994,
1.15847268237915));
#15606=CARTESIAN_POINT('Ctrl Pts',(-0.0452509303920754,0.147607604138013,
1.15582635250005));
#15607=CARTESIAN_POINT('Ctrl Pts',(0.00953524646069181,0.154093252855687,
1.15318002262095));
#15608=CARTESIAN_POINT('Ctrl Pts',(0.0545077808453859,0.136079071706768,
1.15053369274185));
#15609=CARTESIAN_POINT('Ctrl Pts',(0.0994803152300801,0.118064890557849,
1.14788736286275));
#15610=CARTESIAN_POINT('Ctrl Pts',(0.134639207146701,0.0755508795423365,
1.14524103298364));
#15611=CARTESIAN_POINT('Ctrl Pts',(0.14389167861853,0.027996370364851,1.14259470310454));
#15612=CARTESIAN_POINT('Ctrl Pts',(0.15314415009036,-0.0195581388126345,
1.13994837322544));
#15613=CARTESIAN_POINT('Ctrl Pts',(0.136490201117397,-0.0721531461520931,
1.13730204334634));
#15614=CARTESIAN_POINT('Ctrl Pts',(0.101552606157185,-0.105715089329518,
1.13465571346724));
#15615=CARTESIAN_POINT('Ctrl Pts',(0.0666150111969725,-0.139277032506943,
1.13200938358813));
#15616=CARTESIAN_POINT('Ctrl Pts',(0.0133937702495101,-0.153805911522335,
1.12936305370903));
#15617=CARTESIAN_POINT('Ctrl Pts',(-0.033750917386428,-0.142651629870951,
1.12671672382993));
#15618=CARTESIAN_POINT('Ctrl Pts',(-0.0808956050223675,-0.131497348219567,
1.12407039395083));
#15619=CARTESIAN_POINT('Ctrl Pts',(-0.121963739346782,-0.094659905901407,
1.12142406407173));
#15620=CARTESIAN_POINT('Ctrl Pts',(-0.1381577891642,-0.0490003798202082,
1.11877773419262));
#15621=CARTESIAN_POINT('Ctrl Pts',(-0.143690228857438,-0.0334015285560649,
1.11787365765651));
#15622=CARTESIAN_POINT('Ctrl Pts',(-0.146319518115206,-0.0167730178360648,
1.1169695811204));
#15623=CARTESIAN_POINT('Ctrl Pts',(-0.146204073634541,-0.000109175101205505,
1.11606550458429));
#15624=CARTESIAN_POINT('Ctrl Pts',(-0.146170555016798,-9.22629125885076E-5,
1.10893449541571));
#15625=CARTESIAN_POINT('Ctrl Pts',(-0.146275742653821,-0.0183444476975235,
1.10992417600687));
#15626=CARTESIAN_POINT('Ctrl Pts',(-0.143109248288425,-0.0365614514641733,
1.11091385659804));
#15627=CARTESIAN_POINT('Ctrl Pts',(-0.136505188007283,-0.0534328725168923,
1.1119035371892));
#15628=CARTESIAN_POINT('Ctrl Pts',(-0.118839368174718,-0.0985638180183679,
1.11455092656346));
#15629=CARTESIAN_POINT('Ctrl Pts',(-0.0765757310810901,-0.134066323362434,
1.11719831593772));
#15630=CARTESIAN_POINT('Ctrl Pts',(-0.0290731934694857,-0.143678417446031,
1.11984570531198));
#15631=CARTESIAN_POINT('Ctrl Pts',(0.01842934414212,-0.153290511529629,
1.12249309468624));
#15632=CARTESIAN_POINT('Ctrl Pts',(0.071170782271703,-0.137012194352758,
1.1251404840605));
#15633=CARTESIAN_POINT('Ctrl Pts',(0.10499283308901,-0.102299771349957,
1.12778787343476));
#15634=CARTESIAN_POINT('Ctrl Pts',(0.138814883906317,-0.0675873483471558,
1.13043526280902));
#15635=CARTESIAN_POINT('Ctrl Pts',(0.153717547411349,-0.0144408195184256,
1.13308265218328));
#15636=CARTESIAN_POINT('Ctrl Pts',(0.142874638214406,0.0327959749574983,
1.13573004155754));
#15637=CARTESIAN_POINT('Ctrl Pts',(0.132031729017462,0.0800327694334235,
1.1383774309318));
#15638=CARTESIAN_POINT('Ctrl Pts',(0.0954432471185425,0.121359829556542,
1.14102482030606));
#15639=CARTESIAN_POINT('Ctrl Pts',(0.0498685966661331,0.137847238945365,
1.14367220968032));
#15640=CARTESIAN_POINT('Ctrl Pts',(0.00429394621372511,0.154334648334189,
1.14631959905458));
#15641=CARTESIAN_POINT('Ctrl Pts',(-0.0502668727921719,0.145982406988718,
1.14896698842884));
#15642=CARTESIAN_POINT('Ctrl Pts',(-0.0888222026239048,0.116616270474356,
1.1516143778031));
#15643=CARTESIAN_POINT('Ctrl Pts',(-0.124357782404925,0.0895501633622979,
1.1540544170073));
#15644=CARTESIAN_POINT('Ctrl Pts',(-0.146296868742479,0.0446329749882746,
1.15649445621151));
#15645=CARTESIAN_POINT('Ctrl Pts',(-0.146552328192774,-6.73160170860698E-5,
1.15893449541571));
#15646=CARTESIAN_POINT('Origin',(0.,0.,0.));
#15647=CARTESIAN_POINT('',(-0.146318311025392,0.000133437649768732,1.21606550458429));
#15648=CARTESIAN_POINT('',(-0.146373054956946,0.000132657382717961,1.20893449541571));
#15649=CARTESIAN_POINT('',(-0.14635,-1.79227059055215E-17,0.));
#15650=CARTESIAN_POINT('Ctrl Pts',(-0.146318311025392,0.000133437649768732,
1.21606550458429));
#15651=CARTESIAN_POINT('Ctrl Pts',(-0.146429658069886,0.0125190846592594,
1.21539220633629));
#15652=CARTESIAN_POINT('Ctrl Pts',(-0.144988168643405,0.0248791929292086,
1.21471890808829));
#15653=CARTESIAN_POINT('Ctrl Pts',(-0.141892968227885,0.0368102906365087,
1.21404560984029));
#15654=CARTESIAN_POINT('Ctrl Pts',(-0.129727599662405,0.083704249513052,
1.21139927996119));
#15655=CARTESIAN_POINT('Ctrl Pts',(-0.0920156607298113,0.123970842060419,
1.20875295008209));
#15656=CARTESIAN_POINT('Ctrl Pts',(-0.0460184991925076,0.139179415364965,
1.20610662020299));
#15657=CARTESIAN_POINT('Ctrl Pts',(-2.13376552038805E-5,0.15438798866951,
1.20346029032389));
#15658=CARTESIAN_POINT('Ctrl Pts',(0.0542610464868107,0.144538542731236,
1.20081396044478));
#15659=CARTESIAN_POINT('Ctrl Pts',(0.091982751999895,0.114139323915075,
1.19816763056568));
#15660=CARTESIAN_POINT('Ctrl Pts',(0.129704457512977,0.0837401050989159,
1.19552130068658));
#15661=CARTESIAN_POINT('Ctrl Pts',(0.150865484397133,0.0327911134048729,
1.19287497080748));
#15662=CARTESIAN_POINT('Ctrl Pts',(0.145780097726084,-0.0153874961003253,
1.19022864092838));
#15663=CARTESIAN_POINT('Ctrl Pts',(0.140694711055036,-0.063566105605525,
1.18758231104927));
#15664=CARTESIAN_POINT('Ctrl Pts',(0.109362910828785,-0.108974332921877,
1.18493598117017));
#15665=CARTESIAN_POINT('Ctrl Pts',(0.0661257549466402,-0.130828118009858,
1.18228965129107));
#15666=CARTESIAN_POINT('Ctrl Pts',(0.0228885990644955,-0.152681903097838,
1.17964332141197));
#15667=CARTESIAN_POINT('Ctrl Pts',(-0.0322539124735426,-0.150981245957443,
1.17699699153287));
#15668=CARTESIAN_POINT('Ctrl Pts',(-0.0740621845924981,-0.126504564117865,
1.17435066165376));
#15669=CARTESIAN_POINT('Ctrl Pts',(-0.115870456711455,-0.102027882278287,
1.17170433177466));
#15670=CARTESIAN_POINT('Ctrl Pts',(-0.144344489411329,-0.0547751757395235,
1.16905800189556));
#15671=CARTESIAN_POINT('Ctrl Pts',(-0.146451269950206,-0.00637475169995868,
1.16641167201646));
#15672=CARTESIAN_POINT('Ctrl Pts',(-0.146543132875163,-0.00426432565444621,
1.1662962828724));
#15673=CARTESIAN_POINT('Ctrl Pts',(-0.146584864748453,-0.00215171749738942,
1.16618089372835));
#15674=CARTESIAN_POINT('Ctrl Pts',(-0.146577386142569,-3.88073511912723E-5,
1.16606550458429));
#15675=CARTESIAN_POINT('Ctrl Pts',(-0.146552328192774,-6.73160170860698E-5,
1.15893449541571));
#15676=CARTESIAN_POINT('Ctrl Pts',(-0.146574036680232,-0.00386586684592084,
1.15914184558577));
#15677=CARTESIAN_POINT('Ctrl Pts',(-0.1464391612665,-0.00766285139452399,
1.15934919575582));
#15678=CARTESIAN_POINT('Ctrl Pts',(-0.146142739258869,-0.0114471821958193,
1.15955654592588));
#15679=CARTESIAN_POINT('Ctrl Pts',(-0.142358105404532,-0.0597644666683822,
1.16220393530014));
#15680=CARTESIAN_POINT('Ctrl Pts',(-0.112238997038288,-0.106019003930254,
1.1648513246744));
#15681=CARTESIAN_POINT('Ctrl Pts',(-0.0695815129186611,-0.129023839960917,
1.16749871404866));
#15682=CARTESIAN_POINT('Ctrl Pts',(-0.026924028799035,-0.15202867599158,
1.17014610342292));
#15683=CARTESIAN_POINT('Ctrl Pts',(0.0282718310739737,-0.151783810791035,
1.17279349279718));
#15684=CARTESIAN_POINT('Ctrl Pts',(0.0707235276354612,-0.128401405199111,
1.17544088217144));
#15685=CARTESIAN_POINT('Ctrl Pts',(0.11317522419695,-0.105018999607187,
1.1780882715457));
#15686=CARTESIAN_POINT('Ctrl Pts',(0.142882757446916,-0.0584990536238821,
1.18073566091996));
#15687=CARTESIAN_POINT('Ctrl Pts',(0.146238551171451,-0.0101500920973681,
1.18338305029422));
#15688=CARTESIAN_POINT('Ctrl Pts',(0.149594344895986,0.0381988694291446,
1.18603043966848));
#15689=CARTESIAN_POINT('Ctrl Pts',(0.12659839909509,0.0883768464988665,
1.18867782904274));
#15690=CARTESIAN_POINT('Ctrl Pts',(0.0877840381772113,0.117399748124142,
1.191325218417));
#15691=CARTESIAN_POINT('Ctrl Pts',(0.0489696772593311,0.146422649749419,
1.19397260779126));
#15692=CARTESIAN_POINT('Ctrl Pts',(-0.00566309877553352,0.154290475930249,
1.19661999716552));
#15693=CARTESIAN_POINT('Ctrl Pts',(-0.0510896721842483,0.137399358129564,
1.19926738653978));
#15694=CARTESIAN_POINT('Ctrl Pts',(-0.0965162455929618,0.12050824032888,
1.20191477591404));
#15695=CARTESIAN_POINT('Ctrl Pts',(-0.132736616375526,0.0788581785466829,
1.2045621652883));
#15696=CARTESIAN_POINT('Ctrl Pts',(-0.143159994183491,0.0315270405159292,
1.20720955466256));
#15697=CARTESIAN_POINT('Ctrl Pts',(-0.145423823013163,0.021247302336111,
1.20778453491361));
#15698=CARTESIAN_POINT('Ctrl Pts',(-0.146470795531708,0.0106995851133921,
1.20835951516466));
#15699=CARTESIAN_POINT('Ctrl Pts',(-0.146373054956946,0.000132657382717961,
1.20893449541571));
#15700=CARTESIAN_POINT('Origin',(0.,0.,0.));
#15701=CARTESIAN_POINT('',(-0.146120596765396,-4.14129048147555E-5,1.26606550458429));
#15702=CARTESIAN_POINT('',(-0.146109918970638,-1.0198006988139E-5,1.25893449541571));
#15703=CARTESIAN_POINT('',(-0.14635,-1.79227059055215E-17,0.));
#15704=CARTESIAN_POINT('Ctrl Pts',(-0.146120596765396,-4.14129048147555E-5,
1.26606550458429));
#15705=CARTESIAN_POINT('Ctrl Pts',(-0.14605219935785,0.0269443530192317,
1.26460351894424));
#15706=CARTESIAN_POINT('Ctrl Pts',(-0.138898723445843,0.053963836666407,
1.26314153330418));
#15707=CARTESIAN_POINT('Ctrl Pts',(-0.124882896249422,0.0767650581554474,
1.26167954766413));
#15708=CARTESIAN_POINT('Ctrl Pts',(-0.0995129464537159,0.118037388097231,
1.25903321778503));
#15709=CARTESIAN_POINT('Ctrl Pts',(-0.051658938874944,0.145488850208621,
1.25638688790592));
#15710=CARTESIAN_POINT('Ctrl Pts',(-0.00322440565727106,0.146554478394238,
1.25374055802682));
#15711=CARTESIAN_POINT('Ctrl Pts',(0.0452101275604033,0.147620106579856,
1.25109422814772));
#15712=CARTESIAN_POINT('Ctrl Pts',(0.0942251864169787,0.122299900839699,
1.24844789826862));
#15713=CARTESIAN_POINT('Ctrl Pts',(0.121385807331354,0.0821833176976391,
1.24580156838952));
#15714=CARTESIAN_POINT('Ctrl Pts',(0.148546428245729,0.0420667345555804,
1.24315523851041));
#15715=CARTESIAN_POINT('Ctrl Pts',(0.153852611217905,-0.0128462259883804,
1.24050890863131));
#15716=CARTESIAN_POINT('Ctrl Pts',(0.134875632820701,-0.0574210379606392,
1.23786257875221));
#15717=CARTESIAN_POINT('Ctrl Pts',(0.115898654423498,-0.101995849932898,
1.23521624887311));
#15718=CARTESIAN_POINT('Ctrl Pts',(0.0726385146569148,-0.136232513333455,
1.23256991899401));
#15719=CARTESIAN_POINT('Ctrl Pts',(0.0248960600935515,-0.144460368686643,
1.2299235891149));
#15720=CARTESIAN_POINT('Ctrl Pts',(-0.0228463944698117,-0.152688224039831,
1.2272772592358));
#15721=CARTESIAN_POINT('Ctrl Pts',(-0.0750711638299551,-0.134907271345651,
1.2246309293567));
#15722=CARTESIAN_POINT('Ctrl Pts',(-0.107874149410843,-0.0992561323957017,
1.2219845994776));
#15723=CARTESIAN_POINT('Ctrl Pts',(-0.132331163880887,-0.072675612185966,
1.2200115678465));
#15724=CARTESIAN_POINT('Ctrl Pts',(-0.145992019903337,-0.0361614337449312,
1.21803853621539));
#15725=CARTESIAN_POINT('Ctrl Pts',(-0.146318311025392,0.000133437649768732,
1.21606550458429));
#15726=CARTESIAN_POINT('Ctrl Pts',(-0.146373054956946,0.000132657382717961,
1.20893449541571));
#15727=CARTESIAN_POINT('Ctrl Pts',(-0.146020767276673,-0.0379538636644633,
1.21100690453892));
#15728=CARTESIAN_POINT('Ctrl Pts',(-0.130797424420382,-0.0762899498869128,
1.21307931366213));
#15729=CARTESIAN_POINT('Ctrl Pts',(-0.104081054125652,-0.103227285106232,
1.21515172278534));
#15730=CARTESIAN_POINT('Ctrl Pts',(-0.0699523514264828,-0.137638258418326,
1.2177991121596));
#15731=CARTESIAN_POINT('Ctrl Pts',(-0.0170685611947798,-0.153447990763203,
1.22044650153386));
#15732=CARTESIAN_POINT('Ctrl Pts',(0.0303468241642401,-0.143414812629152,
1.22309389090812));
#15733=CARTESIAN_POINT('Ctrl Pts',(0.0777622095232573,-0.133381634495101,
1.22574128028238));
#15734=CARTESIAN_POINT('Ctrl Pts',(0.119709190009594,-0.0975055458821257,
1.22838866965664));
#15735=CARTESIAN_POINT('Ctrl Pts',(0.136973893871985,-0.052219638220276,
1.2310360590309));
#15736=CARTESIAN_POINT('Ctrl Pts',(0.154238597734379,-0.00693373055842239,
1.23368344840516));
#15737=CARTESIAN_POINT('Ctrl Pts',(0.146821024972825,0.0477619961523044,
1.23633083777942));
#15738=CARTESIAN_POINT('Ctrl Pts',(0.118118804930222,0.0868140895256425,
1.23897822715368));
#15739=CARTESIAN_POINT('Ctrl Pts',(0.0894165848876198,0.125866182898978,
1.24162561652794));
#15740=CARTESIAN_POINT('Ctrl Pts',(0.0394297175639698,0.149274642934924,
1.2442730059022));
#15741=CARTESIAN_POINT('Ctrl Pts',(-0.00894524413350711,0.146317192515786,
1.24692039527646));
#15742=CARTESIAN_POINT('Ctrl Pts',(-0.0573202058309854,0.143359742096648,
1.24956778465072));
#15743=CARTESIAN_POINT('Ctrl Pts',(-0.104083261902292,0.114036381222425,
1.25221517402498));
#15744=CARTESIAN_POINT('Ctrl Pts',(-0.127814530591109,0.0717787154251623,
1.25486256339924));
#15745=CARTESIAN_POINT('Ctrl Pts',(-0.139981499518435,0.0501133037087236,
1.2562198740714));
#15746=CARTESIAN_POINT('Ctrl Pts',(-0.146094355379323,0.0250479932723348,
1.25757718474355));
#15747=CARTESIAN_POINT('Ctrl Pts',(-0.146109918970638,-1.0198006988139E-5,
1.25893449541571));
#15748=CARTESIAN_POINT('Origin',(0.,0.,0.));
#15749=CARTESIAN_POINT('',(-0.146470135615938,-0.000111966546850736,1.31606550458429));
#15750=CARTESIAN_POINT('',(-0.146410535958061,-0.000127756381200432,1.30893449541571));
#15751=CARTESIAN_POINT('',(-0.14635,-1.79227059055215E-17,0.));
#15752=CARTESIAN_POINT('Ctrl Pts',(-0.146470135615938,-0.000111966546850736,
1.31606550458429));
#15753=CARTESIAN_POINT('Ctrl Pts',(-0.146120207411574,0.0411799307449602,
1.31381483155218));
#15754=CARTESIAN_POINT('Ctrl Pts',(-0.127827491572984,0.0827431563937987,
1.31156415852007));
#15755=CARTESIAN_POINT('Ctrl Pts',(-0.0969137672218927,0.10998333351997,
1.30931348548796));
#15756=CARTESIAN_POINT('Ctrl Pts',(-0.0605655677022408,0.142012194937238,
1.30666715560886));
#15757=CARTESIAN_POINT('Ctrl Pts',(-0.00676890401288169,0.154239532672684,
1.30402082572976));
#15758=CARTESIAN_POINT('Ctrl Pts',(0.0398526445220406,0.14106870189023,
1.30137449585066));
#15759=CARTESIAN_POINT('Ctrl Pts',(0.0864741930569617,0.127897871107775,
1.29872816597155));
#15760=CARTESIAN_POINT('Ctrl Pts',(0.125920626437448,0.0893288718074177,
1.29608183609245));
#15761=CARTESIAN_POINT('Ctrl Pts',(0.14013669149516,0.0430153417578024,
1.29343550621335));
#15762=CARTESIAN_POINT('Ctrl Pts',(0.154352756552873,-0.00329818829181684,
1.29078917633425));
#15763=CARTESIAN_POINT('Ctrl Pts',(0.143338453287813,-0.0573562490906975,
1.28814284645515));
#15764=CARTESIAN_POINT('Ctrl Pts',(0.112135201594409,-0.0944156157243562,
1.28549651657604));
#15765=CARTESIAN_POINT('Ctrl Pts',(0.0809319499010078,-0.131474982358013,
1.28285018669694));
#15766=CARTESIAN_POINT('Ctrl Pts',(0.0295397497792676,-0.151535654826449,
1.28020385681784));
#15767=CARTESIAN_POINT('Ctrl Pts',(-0.0185183802362589,-0.1454155477333,
1.27755752693874));
#15768=CARTESIAN_POINT('Ctrl Pts',(-0.066576510251784,-0.139295440640151,
1.27491119705964));
#15769=CARTESIAN_POINT('Ctrl Pts',(-0.111300570161094,-0.106994553985419,
1.27226486718053));
#15770=CARTESIAN_POINT('Ctrl Pts',(-0.13221965410943,-0.0632975117719662,
1.26961853730143));
#15771=CARTESIAN_POINT('Ctrl Pts',(-0.141581826511298,-0.0437412423069929,
1.26843419306239));
#15772=CARTESIAN_POINT('Ctrl Pts',(-0.146176005022067,-0.0219023912433209,
1.26724984882334));
#15773=CARTESIAN_POINT('Ctrl Pts',(-0.146120596765396,-4.14129048147555E-5,
1.26606550458429));
#15774=CARTESIAN_POINT('Ctrl Pts',(-0.146109918970638,-1.0198006988139E-5,
1.25893449541571));
#15775=CARTESIAN_POINT('Ctrl Pts',(-0.146124711647138,-0.0238271763493914,
1.26022457411781));
#15776=CARTESIAN_POINT('Ctrl Pts',(-0.140631289159497,-0.0476377233371588,
1.26151465281992));
#15777=CARTESIAN_POINT('Ctrl Pts',(-0.129592576141605,-0.0685164391025303,
1.26280473152202));
#15778=CARTESIAN_POINT('Ctrl Pts',(-0.106939871696956,-0.111361957112663,
1.26545212089628));
#15779=CARTESIAN_POINT('Ctrl Pts',(-0.0609349815013302,-0.141861022412626,
1.26809951027054));
#15780=CARTESIAN_POINT('Ctrl Pts',(-0.0126505083952331,-0.146043496451057,
1.2707468996448));
#15781=CARTESIAN_POINT('Ctrl Pts',(0.0356339647108625,-0.150225970489488,
1.27339428901906));
#15782=CARTESIAN_POINT('Ctrl Pts',(0.0861980207274291,-0.128091853266388,
1.27604167839332));
#15783=CARTESIAN_POINT('Ctrl Pts',(0.11588072467734,-0.0897797074320025,
1.27868906776758));
#15784=CARTESIAN_POINT('Ctrl Pts',(0.145563428627253,-0.0514675615976161,
1.28133645714184));
#15785=CARTESIAN_POINT('Ctrl Pts',(0.154364780510509,0.00302261284805656,
1.2839838465161));
#15786=CARTESIAN_POINT('Ctrl Pts',(0.138253309066183,0.0487315170146188,
1.28663123589036));
#15787=CARTESIAN_POINT('Ctrl Pts',(0.122141837621857,0.0944404211811797,
1.28927862526462));
#15788=CARTESIAN_POINT('Ctrl Pts',(0.0811175428499519,0.131368055068631,
1.29192601463888));
#15789=CARTESIAN_POINT('Ctrl Pts',(0.0339716590485425,0.142599665496764,
1.29457340401314));
#15790=CARTESIAN_POINT('Ctrl Pts',(-0.013174224752867,0.153831275924897,
1.2972207933874));
#15791=CARTESIAN_POINT('Ctrl Pts',(-0.0664416975837803,0.139366862893713,
1.29986818276166));
#15792=CARTESIAN_POINT('Ctrl Pts',(-0.101431520699135,0.105831870563862,
1.30251557213592));
#15793=CARTESIAN_POINT('Ctrl Pts',(-0.129710573305276,0.0787286237393239,
1.30465521322918));
#15794=CARTESIAN_POINT('Ctrl Pts',(-0.146050663974784,0.0391684733249047,
1.30679485432245));
#15795=CARTESIAN_POINT('Ctrl Pts',(-0.146410535958061,-0.000127756381200432,
1.30893449541571));
#15796=CARTESIAN_POINT('Origin',(0.,0.,0.));
#15797=CARTESIAN_POINT('',(-0.146471469669193,0.000111495080380188,1.36606550458429));
#15798=CARTESIAN_POINT('',(-0.146526884620975,8.5711493927648E-5,1.35893449541571));
#15799=CARTESIAN_POINT('',(-0.14635,-1.79227059055215E-17,0.));
#15800=CARTESIAN_POINT('Ctrl Pts',(-0.146471469669193,0.000111495080380188,
1.36606550458429));
#15801=CARTESIAN_POINT('Ctrl Pts',(-0.146532402405025,0.0073220458586883,
1.36567247403923));
#15802=CARTESIAN_POINT('Ctrl Pts',(-0.146045973070864,0.0145243451116175,
1.36527944349416));
#15803=CARTESIAN_POINT('Ctrl Pts',(-0.144983764805735,0.0216407019395156,
1.3648864129491));
#15804=CARTESIAN_POINT('Ctrl Pts',(-0.137831767320671,0.0695561322809842,
1.36224008307));
#15805=CARTESIAN_POINT('Ctrl Pts',(-0.104576727819841,0.113575347233418,
1.3595937531909));
#15806=CARTESIAN_POINT('Ctrl Pts',(-0.060440002550743,0.133550058215342,
1.3569474233118));
#15807=CARTESIAN_POINT('Ctrl Pts',(-0.0163032772816473,0.153524769197265,
1.35430109343269));
#15808=CARTESIAN_POINT('Ctrl Pts',(0.0387151337557165,0.149454976208681,
1.35165476355359));
#15809=CARTESIAN_POINT('Ctrl Pts',(0.0794324390145508,0.123203488242689,
1.34900843367449));
#15810=CARTESIAN_POINT('Ctrl Pts',(0.120149744273387,0.0969520002766962,
1.34636210379539));
#15811=CARTESIAN_POINT('Ctrl Pts',(0.146565943753694,0.048518817333291,
1.34371577391629));
#15812=CARTESIAN_POINT('Ctrl Pts',(0.14658992694451,7.25688577880009E-5,
1.34106944403718));
#15813=CARTESIAN_POINT('Ctrl Pts',(0.146613910135327,-0.0483736796177136,
1.33842311415808));
#15814=CARTESIAN_POINT('Ctrl Pts',(0.120245677036657,-0.0968329936253116,
1.33577678427898));
#15815=CARTESIAN_POINT('Ctrl Pts',(0.0795543829983497,-0.123124782547022,
1.33313045439988));
#15816=CARTESIAN_POINT('Ctrl Pts',(0.0388630889600415,-0.149416571468734,
1.33048412452078));
#15817=CARTESIAN_POINT('Ctrl Pts',(-0.0161512660179049,-0.153540835304554,
1.32783779464168));
#15818=CARTESIAN_POINT('Ctrl Pts',(-0.0603077462478081,-0.133609833714981,
1.32519146476257));
#15819=CARTESIAN_POINT('Ctrl Pts',(-0.10446422647771,-0.113678832125408,
1.32254513488347));
#15820=CARTESIAN_POINT('Ctrl Pts',(-0.137762831959571,-0.0696925651104417,
1.31989880500437));
#15821=CARTESIAN_POINT('Ctrl Pts',(-0.144962267025529,-0.0217842390534145,
1.31725247512527));
#15822=CARTESIAN_POINT('Ctrl Pts',(-0.146038665626028,-0.0146213916011371,
1.31685681827827));
#15823=CARTESIAN_POINT('Ctrl Pts',(-0.146531651210624,-0.00737087161912708,
1.31646116143128));
#15824=CARTESIAN_POINT('Ctrl Pts',(-0.146470135615938,-0.000111966546850736,
1.31606550458429));
#15825=CARTESIAN_POINT('Ctrl Pts',(-0.146410535958061,-0.000127756381200432,
1.30893449541571));
#15826=CARTESIAN_POINT('Ctrl Pts',(-0.146495935505426,-0.00945296197092968,
1.30944224369671));
#15827=CARTESIAN_POINT('Ctrl Pts',(-0.145681427739287,-0.018763305174839,
1.3099499919777));
#15828=CARTESIAN_POINT('Ctrl Pts',(-0.143913007029536,-0.0278887903271487,
1.3104577402587));
#15829=CARTESIAN_POINT('Ctrl Pts',(-0.134692496844786,-0.0754688872597875,
1.31310512963296));
#15830=CARTESIAN_POINT('Ctrl Pts',(-0.0995393030754929,-0.118023509496548,
1.31575251900722));
#15831=CARTESIAN_POINT('Ctrl Pts',(-0.0545553941775042,-0.136060454153345,
1.31839990838148));
#15832=CARTESIAN_POINT('Ctrl Pts',(-0.00957148527951295,-0.154097398810142,
1.32104729775574));
#15833=CARTESIAN_POINT('Ctrl Pts',(0.0452431387471776,-0.14761666588697,
1.32369468713));
#15834=CARTESIAN_POINT('Ctrl Pts',(0.0847805644327026,-0.119586763955155,
1.32634207650426));
#15835=CARTESIAN_POINT('Ctrl Pts',(0.124317990118227,-0.09155686202334,
1.32898946587852));
#15836=CARTESIAN_POINT('Ctrl Pts',(0.148578217462589,-0.041977791082884,
1.33163685525278));
#15837=CARTESIAN_POINT('Ctrl Pts',(0.146448816178573,0.00644068764408242,
1.33428424462704));
#15838=CARTESIAN_POINT('Ctrl Pts',(0.144319414894557,0.0548591663710502,
1.3369316340013));
#15839=CARTESIAN_POINT('Ctrl Pts',(0.115800384982161,0.102117052884526,
1.33957902337556));
#15840=CARTESIAN_POINT('Ctrl Pts',(0.0739549070570988,0.126567807678519,
1.34222641274982));
#15841=CARTESIAN_POINT('Ctrl Pts',(0.0321094291320376,0.151018562472512,
1.34487380212408));
#15842=CARTESIAN_POINT('Ctrl Pts',(-0.0230624968056921,0.152662185547021,
1.34752119149834));
#15843=CARTESIAN_POINT('Ctrl Pts',(-0.0662892946253695,0.1307458130856,
1.3501685808726));
#15844=CARTESIAN_POINT('Ctrl Pts',(-0.109516092445046,0.10882944062418,
1.35281597024686));
#15845=CARTESIAN_POINT('Ctrl Pts',(-0.140797762146673,0.0633530726268328,
1.35546335962112));
#15846=CARTESIAN_POINT('Ctrl Pts',(-0.145805692234247,0.0151472216574969,
1.35811074899538));
#15847=CARTESIAN_POINT('Ctrl Pts',(-0.146325105122407,0.0101474034011793,
1.35838533113549));
#15848=CARTESIAN_POINT('Ctrl Pts',(-0.146561879835735,0.00511822289583405,
1.3586599132756));
#15849=CARTESIAN_POINT('Ctrl Pts',(-0.146526884620975,8.5711493927648E-5,
1.35893449541571));
#15850=CARTESIAN_POINT('Origin',(0.,0.,0.));
#15851=CARTESIAN_POINT('',(-0.146120987371435,4.2191387702159E-5,1.41606550458429));
#15852=CARTESIAN_POINT('',(-0.146148882937928,7.6306569664006E-5,1.40893449541571));
#15853=CARTESIAN_POINT('',(-0.14635,-1.79227059055215E-17,0.));
#15854=CARTESIAN_POINT('Ctrl Pts',(-0.146120987371435,4.2191387702159E-5,
1.41606550458429));
#15855=CARTESIAN_POINT('Ctrl Pts',(-0.146177309023295,0.021854523983563,
1.41488378664717));
#15856=CARTESIAN_POINT('Ctrl Pts',(-0.141604359564088,0.0436444172696427,
1.41370206871005));
#15857=CARTESIAN_POINT('Ctrl Pts',(-0.132282279973341,0.0631665524487371,
1.41252035077294));
#15858=CARTESIAN_POINT('Ctrl Pts',(-0.1114064880593,0.106884268839086,1.40987402089383));
#15859=CARTESIAN_POINT('Ctrl Pts',(-0.0667143915920224,0.139229456738304,
1.40722769101473));
#15860=CARTESIAN_POINT('Ctrl Pts',(-0.0186623352932378,0.145397151366753,
1.40458136113563));
#15861=CARTESIAN_POINT('Ctrl Pts',(0.0293897210055454,0.151564845995202,
1.40193503125653));
#15862=CARTESIAN_POINT('Ctrl Pts',(0.0808017371358351,0.131555047352884,
1.39928870137743));
#15863=CARTESIAN_POINT('Ctrl Pts',(0.112041660826149,0.0945265884816804,
1.39664237149832));
#15864=CARTESIAN_POINT('Ctrl Pts',(0.143281584516463,0.0574981296104763,
1.39399604161922));
#15865=CARTESIAN_POINT('Ctrl Pts',(0.154349415766802,0.00345101051038574,
1.39134971174012));
#15866=CARTESIAN_POINT('Ctrl Pts',(0.140179214932283,-0.0428765696854336,
1.38870338186102));
#15867=CARTESIAN_POINT('Ctrl Pts',(0.126009014097764,-0.089204149881253,
1.38605705198192));
#15868=CARTESIAN_POINT('Ctrl Pts',(0.0866007811783877,-0.127812191172801,
1.38341072210282));
#15869=CARTESIAN_POINT('Ctrl Pts',(0.0399922944706322,-0.14102917638501,
1.38076439222371));
#15870=CARTESIAN_POINT('Ctrl Pts',(-0.00661619223712474,-0.15424616159722,
1.37811806234461));
#15871=CARTESIAN_POINT('Ctrl Pts',(-0.060424932733261,-0.142072090730089,
1.37547173246551));
#15872=CARTESIAN_POINT('Ctrl Pts',(-0.0968048252466797,-0.110079232431271,
1.37282540258641));
#15873=CARTESIAN_POINT('Ctrl Pts',(-0.127781608685608,-0.08283792481198,
1.37057210325237));
#15874=CARTESIAN_POINT('Ctrl Pts',(-0.146122133733866,-0.0412276055847571,
1.36831880391833));
#15875=CARTESIAN_POINT('Ctrl Pts',(-0.146471469669193,0.000111495080380188,
1.36606550458429));
#15876=CARTESIAN_POINT('Ctrl Pts',(-0.146526884620975,8.5711493927648E-5,
1.35893449541571));
#15877=CARTESIAN_POINT('Ctrl Pts',(-0.146224472749943,-0.0434028397118431,
1.36130730264986));
#15878=CARTESIAN_POINT('Ctrl Pts',(-0.125627402569456,-0.0871401285467012,
1.36368010988401));
#15879=CARTESIAN_POINT('Ctrl Pts',(-0.0917490966422633,-0.114327780902106,
1.36605291711816));
#15880=CARTESIAN_POINT('Ctrl Pts',(-0.0539503804891888,-0.144661598551044,
1.36870030649242));
#15881=CARTESIAN_POINT('Ctrl Pts',(0.00038124229047478,-0.154393899907594,
1.37134769586668));
#15882=CARTESIAN_POINT('Ctrl Pts',(0.0463590973565905,-0.139066790892088,
1.37399508524094));
#15883=CARTESIAN_POINT('Ctrl Pts',(0.0923369524227062,-0.123739681876581,
1.3766424746152));
#15884=CARTESIAN_POINT('Ctrl Pts',(0.129961039775272,-0.083353162489017,
1.37928986398946));
#15885=CARTESIAN_POINT('Ctrl Pts',(0.141997595260484,-0.0364063334065561,
1.38193725336372));
#15886=CARTESIAN_POINT('Ctrl Pts',(0.154034150745695,0.0105404956759021,
1.38458464273798));
#15887=CARTESIAN_POINT('Ctrl Pts',(0.140483174363557,0.0640476344532581,
1.38723203211224));
#15888=CARTESIAN_POINT('Ctrl Pts',(0.10755170844225,0.0996060653705087,
1.3898794214865));
#15889=CARTESIAN_POINT('Ctrl Pts',(0.0746202425209409,0.135164496287762,
1.39252681086076));
#15890=CARTESIAN_POINT('Ctrl Pts',(0.0223082870604623,0.152774219344908,
1.39517420023502));
#15891=CARTESIAN_POINT('Ctrl Pts',(-0.025422593472234,0.144369075867769,
1.39782158960928));
#15892=CARTESIAN_POINT('Ctrl Pts',(-0.073153474004929,0.135963932390631,
1.40046897898354));
#15893=CARTESIAN_POINT('Ctrl Pts',(-0.11630327960984,0.101543922379208,
1.4031163683578));
#15894=CARTESIAN_POINT('Ctrl Pts',(-0.135107186188192,0.0568751802851974,
1.40576375773206));
#15895=CARTESIAN_POINT('Ctrl Pts',(-0.142614236437708,0.0390421576584788,
1.40682067029328));
#15896=CARTESIAN_POINT('Ctrl Pts',(-0.14624095998336,0.0195756595648056,
1.40787758285449));
#15897=CARTESIAN_POINT('Ctrl Pts',(-0.146148882937928,7.6306569664006E-5,
1.40893449541571));
#15898=CARTESIAN_POINT('Origin',(0.,0.,0.));
#15899=CARTESIAN_POINT('',(-0.14631473222987,-0.000131398079681141,1.46606550458429));
#15900=CARTESIAN_POINT('',(-0.146248097568756,-0.000123763188177425,1.45893449541571));
#15901=CARTESIAN_POINT('',(-0.14635,-1.79227059055215E-17,0.));
#15902=CARTESIAN_POINT('Ctrl Pts',(-0.14631473222987,-0.000131398079681141,
1.46606550458429));
#15903=CARTESIAN_POINT('Ctrl Pts',(-0.145989697979493,0.0361157155227289,
1.46409509925512));
#15904=CARTESIAN_POINT('Ctrl Pts',(-0.132370868650209,0.0725796635271419,
1.46212469392594));
#15905=CARTESIAN_POINT('Ctrl Pts',(-0.107973319296019,0.0991484059484618,
1.46015428859677));
#15906=CARTESIAN_POINT('Ctrl Pts',(-0.0752064754000165,0.134831245351468,
1.45750795871767));
#15907=CARTESIAN_POINT('Ctrl Pts',(-0.0229974942306327,0.152665588379184,
1.45486162883857));
#15908=CARTESIAN_POINT('Ctrl Pts',(0.0247535192036911,0.144485406820094,
1.45221529895946));
#15909=CARTESIAN_POINT('Ctrl Pts',(0.0725045326380122,0.136305225261004,
1.44956896908036));
#15910=CARTESIAN_POINT('Ctrl Pts',(0.115797578337275,0.102110519115111,
1.44692263920126));
#15911=CARTESIAN_POINT('Ctrl Pts',(0.134818450998255,0.0575543070937695,
1.44427630932216));
#15912=CARTESIAN_POINT('Ctrl Pts',(0.153839323659235,0.0129980950724284,
1.44162997944306));
#15913=CARTESIAN_POINT('Ctrl Pts',(0.148588023281934,-0.0419196228243577,
1.43898364956396));
#15914=CARTESIAN_POINT('Ctrl Pts',(0.121467255745355,-0.082062966762292,
1.43633731968485));
#15915=CARTESIAN_POINT('Ctrl Pts',(0.0943464882087764,-0.122206310700226,
1.43369098980575));
#15916=CARTESIAN_POINT('Ctrl Pts',(0.0453562535129183,-0.147575280679306,
1.43104465992665));
#15917=CARTESIAN_POINT('Ctrl Pts',(-0.00307937473935208,-0.146557666176543,
1.42839833004755));
#15918=CARTESIAN_POINT('Ctrl Pts',(-0.0515150029916225,-0.14554005167378,
1.42575200016845));
#15919=CARTESIAN_POINT('Ctrl Pts',(-0.0993960248003067,-0.118135852689175,
1.42310567028934));
#15920=CARTESIAN_POINT('Ctrl Pts',(-0.124806792024246,-0.0768886307561326,
1.42045934041024));
#15921=CARTESIAN_POINT('Ctrl Pts',(-0.138870387581649,-0.0540603453281256,
1.41899472846826));
#15922=CARTESIAN_POINT('Ctrl Pts',(-0.146051182757901,-0.0269918425378075,
1.41753011652627));
#15923=CARTESIAN_POINT('Ctrl Pts',(-0.146120987371435,4.2191387702159E-5,
1.41606550458429));
#15924=CARTESIAN_POINT('Ctrl Pts',(-0.146148882937928,7.6306569664006E-5,
1.40893449541571));
#15925=CARTESIAN_POINT('Ctrl Pts',(-0.146010322369016,-0.0292669616874671,
1.41052497222875));
#15926=CARTESIAN_POINT('Ctrl Pts',(-0.137450455640384,-0.0586846305953837,
1.4121154490418));
#15927=CARTESIAN_POINT('Ctrl Pts',(-0.121019719714466,-0.0827222215753489,
1.41370592585484));
#15928=CARTESIAN_POINT('Ctrl Pts',(-0.0936703391105966,-0.122733407165291,
1.4163533152291));
#15929=CARTESIAN_POINT('Ctrl Pts',(-0.0445135703510636,-0.147838304168576,
1.41900070460336));
#15930=CARTESIAN_POINT('Ctrl Pts',(0.00393424939099551,-0.146537573651384,
1.42164809397762));
#15931=CARTESIAN_POINT('Ctrl Pts',(0.0523820691330518,-0.145236843134192,
1.42429548335188));
#15932=CARTESIAN_POINT('Ctrl Pts',(0.100120939857634,-0.117530485096527,
1.42694287272614));
#15933=CARTESIAN_POINT('Ctrl Pts',(0.125284029446909,-0.0761094471358441,
1.4295902621004));
#15934=CARTESIAN_POINT('Ctrl Pts',(0.150447119036187,-0.0346884091751576,
1.43223765147466));
#15935=CARTESIAN_POINT('Ctrl Pts',(0.153034427490153,0.020447308708549,
1.43488504084892));
#15936=CARTESIAN_POINT('Ctrl Pts',(0.13186079120536,0.0640427391611241,
1.43753243022318));
#15937=CARTESIAN_POINT('Ctrl Pts',(0.110687154920568,0.107638169613697,
1.44017981959744));
#15938=CARTESIAN_POINT('Ctrl Pts',(0.0657525738970213,0.139693312635139,
1.4428272089717));
#15939=CARTESIAN_POINT('Ctrl Pts',(0.0176394768514684,0.145525221357757,
1.44547459834596));
#15940=CARTESIAN_POINT('Ctrl Pts',(-0.0304736201940859,0.151357130080375,
1.44812198772022));
#15941=CARTESIAN_POINT('Ctrl Pts',(-0.0817652332616461,0.130965804504167,
1.45076937709448));
#15942=CARTESIAN_POINT('Ctrl Pts',(-0.112741325423428,0.0936916042199666,
1.45341676646874));
#15943=CARTESIAN_POINT('Ctrl Pts',(-0.134261605244105,0.0677957870194472,
1.45525600945106));
#15944=CARTESIAN_POINT('Ctrl Pts',(-0.145976367207401,0.0337512577971725,
1.45709525243339));
#15945=CARTESIAN_POINT('Ctrl Pts',(-0.146248097568756,-0.000123763188177425,
1.45893449541571));
#15946=CARTESIAN_POINT('Origin',(0.,0.,-0.0924367114736175));
#15947=CARTESIAN_POINT('',(-0.117746618301147,-0.000105742458702955,1.48256328852638));
#15948=CARTESIAN_POINT('',(-0.117971241274414,-5.28325160115065E-6,1.49243671147361));
#15949=CARTESIAN_POINT('',(-0.117775,2.85464118895969E-14,-0.0924367114736175));
#15950=CARTESIAN_POINT('',(-0.117668597464313,0.00500517689812599,1.532225));
#15951=CARTESIAN_POINT('Ctrl Pts',(-0.117746618301147,-0.000105742458702949,
1.48256328852638));
#15952=CARTESIAN_POINT('Ctrl Pts',(-0.117836347163251,-0.0101121102621826,
1.48323921307631));
#15953=CARTESIAN_POINT('Ctrl Pts',(-0.112089674709738,-0.0591937430214443,
1.48656146750534));
#15954=CARTESIAN_POINT('Ctrl Pts',(-0.0435804807853106,-0.132222740314769,
1.49253005181348));
#15955=CARTESIAN_POINT('Ctrl Pts',(0.0874774386997331,-0.108286040948335,
1.50046904145078));
#15956=CARTESIAN_POINT('Ctrl Pts',(0.138385550162814,0.0147146982980264,
1.50840803108809));
#15957=CARTESIAN_POINT('Ctrl Pts',(0.0627460642121078,0.124368470664037,
1.51634702072539));
#15958=CARTESIAN_POINT('Ctrl Pts',(-0.0706026869052757,0.119928391791904,
1.5242860103627));
#15959=CARTESIAN_POINT('Ctrl Pts',(-0.116004137797729,0.0441355889673283,
1.5295786701209));
#15960=CARTESIAN_POINT('Ctrl Pts',(-0.117668597464313,0.00500517689812487,
1.532225));
#15961=CARTESIAN_POINT('',(-0.0334019664627544,0.1129391839063,1.53222500000001));
#15962=CARTESIAN_POINT('Origin',(0.,0.,1.532225));
#15963=CARTESIAN_POINT('Ctrl Pts',(-0.117971276761593,-5.28420699491729E-6,
1.49243671147361));
#15964=CARTESIAN_POINT('Ctrl Pts',(-0.117971582784674,-0.000385634193345565,
1.49246252744444));
#15965=CARTESIAN_POINT('Ctrl Pts',(-0.117794795258817,-0.0397700451254522,
1.49513573278954));
#15966=CARTESIAN_POINT('Ctrl Pts',(-0.0742871760264013,-0.117748889605885,
1.50045632750888));
#15967=CARTESIAN_POINT('Ctrl Pts',(0.0586284551779338,-0.126233948370975,
1.50839849563167));
#15968=CARTESIAN_POINT('Ctrl Pts',(0.137995068118234,-0.019163470063063,
1.51634066375444));
#15969=CARTESIAN_POINT('Ctrl Pts',(0.0906261803825392,0.105639137646141,
1.52428283187723));
#15970=CARTESIAN_POINT('Ctrl Pts',(0.00417072711528833,0.124051375507138,
1.52957761062575));
#15971=CARTESIAN_POINT('Ctrl Pts',(-0.0334019664627544,0.1129391839063,
1.53222500000001));
#15972=CARTESIAN_POINT('Origin',(0.,0.,-0.0924367114736175));
#15973=CARTESIAN_POINT('',(-0.117590702341447,3.3953472435133E-5,1.43256328852638));
#15974=CARTESIAN_POINT('',(-0.117692994131604,-9.95982882293356E-5,1.44243671147361));
#15975=CARTESIAN_POINT('',(-0.117775,2.85464118895969E-14,-0.0924367114736175));
#15976=CARTESIAN_POINT('Ctrl Pts',(-0.117590702341447,3.39534724351446E-5,
1.43256328852638));
#15977=CARTESIAN_POINT('Ctrl Pts',(-0.117534527156218,-0.0217216553118358,
1.43402790046837));
#15978=CARTESIAN_POINT('Ctrl Pts',(-0.101314495966545,-0.0828641818343832,
1.43813884228945));
#15979=CARTESIAN_POINT('Ctrl Pts',(-0.00292444232197888,-0.139176693688359,
1.44489611398964));
#15980=CARTESIAN_POINT('Ctrl Pts',(0.115350068603298,-0.0779297424218237,
1.45283510362695));
#15981=CARTESIAN_POINT('Ctrl Pts',(0.128028003046829,0.0546551750765237,
1.46077409326425));
#15982=CARTESIAN_POINT('Ctrl Pts',(0.0235079116789307,0.137209630484779,
1.46871308290156));
#15983=CARTESIAN_POINT('Ctrl Pts',(-0.0918059616614023,0.0978189523496558,
1.47597614798894));
#15984=CARTESIAN_POINT('Ctrl Pts',(-0.117485047349053,0.0290640819657798,
1.48059288319721));
#15985=CARTESIAN_POINT('Ctrl Pts',(-0.117746618301147,-0.000105742458702949,
1.48256328852638));
#15986=CARTESIAN_POINT('Ctrl Pts',(-0.117692994131604,-9.9598288229346E-5,
1.44243671147361));
#15987=CARTESIAN_POINT('Ctrl Pts',(-0.117789077779518,-0.0120777797952868,
1.44324485786555));
#15988=CARTESIAN_POINT('Ctrl Pts',(-0.110597905189529,-0.0631824179582176,
1.44670039363175));
#15989=CARTESIAN_POINT('Ctrl Pts',(-0.0368790902657646,-0.134252921254984,
1.45280331877221));
#15990=CARTESIAN_POINT('Ctrl Pts',(0.0928396680879532,-0.103751556080299,
1.46074548689499));
#15991=CARTESIAN_POINT('Ctrl Pts',(0.137511141307062,0.0217950526079239,
1.46868765501776));
#15992=CARTESIAN_POINT('Ctrl Pts',(0.0562018483347667,0.127378648737854,
1.47662982314055));
#15993=CARTESIAN_POINT('Ctrl Pts',(-0.0761502833827582,0.1162998103107,
1.48454617529249));
#15994=CARTESIAN_POINT('Ctrl Pts',(-0.117940200573233,0.0386186906477724,
1.48981513807018));
#15995=CARTESIAN_POINT('Ctrl Pts',(-0.117971276761593,-5.28420699491729E-6,
1.49243671147361));
#15996=CARTESIAN_POINT('Origin',(0.,0.,-0.0924367114736175));
#15997=CARTESIAN_POINT('',(-0.117872752581409,8.97255421561373E-5,1.38256328852638));
#15998=CARTESIAN_POINT('',(-0.117613151267609,6.14076272390171E-5,1.39243671147361));
#15999=CARTESIAN_POINT('',(-0.117775,2.85464118895969E-14,-0.0924367114736175));
#16000=CARTESIAN_POINT('Ctrl Pts',(-0.117872752581409,8.97255421561322E-5,
1.38256328852638));
#16001=CARTESIAN_POINT('Ctrl Pts',(-0.117591624875346,-0.0331778698171688,
1.38481658786042));
#16002=CARTESIAN_POINT('Ctrl Pts',(-0.0854981695600773,-0.105990339321694,
1.38971621707357));
#16003=CARTESIAN_POINT('Ctrl Pts',(0.0379781508110965,-0.133926497290667,
1.39726217616581));
#16004=CARTESIAN_POINT('Ctrl Pts',(0.133119345865688,-0.0407171622080862,
1.40520116580311));
#16005=CARTESIAN_POINT('Ctrl Pts',(0.106398871137127,0.0897659150453452,
1.41314015544042));
#16006=CARTESIAN_POINT('Ctrl Pts',(-0.0177224175491345,0.138074504763813,
1.42107914507772));
#16007=CARTESIAN_POINT('Ctrl Pts',(-0.105714817800915,0.0743914165933911,
1.42755352277305));
#16008=CARTESIAN_POINT('Ctrl Pts',(-0.11763602712824,0.0175874039095825,
1.43138157058926));
#16009=CARTESIAN_POINT('Ctrl Pts',(-0.117590702341447,3.39534724351446E-5,
1.43256328852638));
#16010=CARTESIAN_POINT('Ctrl Pts',(-0.117613151267609,6.1407627239024E-5,
1.39243671147361));
#16011=CARTESIAN_POINT('Ctrl Pts',(-0.117501644803633,-0.0235525549213426,
1.39402718828666));
#16012=CARTESIAN_POINT('Ctrl Pts',(-0.0991469449676741,-0.0866320980727062,
1.39826505447396));
#16013=CARTESIAN_POINT('Ctrl Pts',(0.00373660876362508,-0.139175849115243,
1.40515031003553));
#16014=CARTESIAN_POINT('Ctrl Pts',(0.118990018389619,-0.0722858665142316,
1.41309247815831));
#16015=CARTESIAN_POINT('Ctrl Pts',(0.125236419206141,0.0608253567263532,
1.42103464628109));
#16016=CARTESIAN_POINT('Ctrl Pts',(0.0167532566496359,0.13821437898841,
1.42897681440387));
#16017=CARTESIAN_POINT('Ctrl Pts',(-0.0944771051913143,0.0939940009069027,
1.43611083613471));
#16018=CARTESIAN_POINT('Ctrl Pts',(-0.117474319425011,0.0271612872365273,
1.44059746849129));
#16019=CARTESIAN_POINT('Ctrl Pts',(-0.117692994131604,-9.9598288229346E-5,
1.44243671147361));
#16020=CARTESIAN_POINT('Origin',(0.,0.,-0.0924367114736175));
#16021=CARTESIAN_POINT('',(-0.117871679003533,-9.01049542302267E-5,1.33256328852638));
#16022=CARTESIAN_POINT('',(-0.117917347702326,6.89762296073142E-5,1.34243671147361));
#16023=CARTESIAN_POINT('',(-0.117775,2.85464118895969E-14,-0.0924367114736175));
#16024=CARTESIAN_POINT('Ctrl Pts',(-0.117871679003533,-9.01049542302501E-5,
1.33256328852638));
#16025=CARTESIAN_POINT('Ctrl Pts',(-0.117921183610054,-0.00593170075121234,
1.33295894537338));
#16026=CARTESIAN_POINT('Ctrl Pts',(-0.114870949065289,-0.0507926200311143,
1.33600093209947));
#16027=CARTESIAN_POINT('Ctrl Pts',(-0.0572704544775333,-0.126880813469472,
1.34168924870467));
#16028=CARTESIAN_POINT('Ctrl Pts',(0.0755477687720905,-0.116923823242002,
1.34962823834197));
#16029=CARTESIAN_POINT('Ctrl Pts',(0.13920718769651,6.89141801743488E-5,
1.35756722797928));
#16030=CARTESIAN_POINT('Ctrl Pts',(0.0754319660950179,0.116998564767658,
1.36550621761658));
#16031=CARTESIAN_POINT('Ctrl Pts',(-0.0573960494825499,0.126824048933643,
1.37344520725389));
#16032=CARTESIAN_POINT('Ctrl Pts',(-0.11489462347839,0.0507140179075799,
1.37913089755716));
#16033=CARTESIAN_POINT('Ctrl Pts',(-0.117921788132912,0.00589240827474643,
1.38217025798132));
#16034=CARTESIAN_POINT('Ctrl Pts',(-0.117872752581409,8.97255421561322E-5,
1.38256328852638));
#16035=CARTESIAN_POINT('Ctrl Pts',(-0.117917347702326,6.89762296073276E-5,
1.34243671147361));
#16036=CARTESIAN_POINT('Ctrl Pts',(-0.117673982084908,-0.0349283870656527,
1.34480951870776));
#16037=CARTESIAN_POINT('Ctrl Pts',(-0.0826049238592893,-0.109396528181867,
1.34982971531618));
#16038=CARTESIAN_POINT('Ctrl Pts',(0.0440301174146577,-0.132080378229483,
1.35749730129884));
#16039=CARTESIAN_POINT('Ctrl Pts',(0.13486394497766,-0.0345773583278084,
1.36543946942163));
#16040=CARTESIAN_POINT('Ctrl Pts',(0.102148545386143,0.0946020732301706,
1.3733816375444));
#16041=CARTESIAN_POINT('Ctrl Pts',(-0.0241454188302812,0.137116288461919,
1.38132380566719));
#16042=CARTESIAN_POINT('Ctrl Pts',(-0.107458038693719,0.07065895059964,
1.38767549697692));
#16043=CARTESIAN_POINT('Ctrl Pts',(-0.117687250167678,0.015753490298928,
1.3913797989124));
#16044=CARTESIAN_POINT('Ctrl Pts',(-0.117613151267609,6.1407627239024E-5,
1.39243671147361));
#16045=CARTESIAN_POINT('Origin',(0.,0.,-0.0924367114736175));
#16046=CARTESIAN_POINT('',(-0.117590388001671,-3.33269891443968E-5,1.28256328852638));
#16047=CARTESIAN_POINT('',(-0.117823716245033,-0.000102811805890834,1.29243671147362));
#16048=CARTESIAN_POINT('',(-0.117775,2.85464118895969E-14,-0.0924367114736175));
#16049=CARTESIAN_POINT('Ctrl Pts',(-0.117590388001671,-3.33269891444124E-5,
1.28256328852638));
#16050=CARTESIAN_POINT('Ctrl Pts',(-0.117634977734708,-0.017625925033684,
1.28374763276543));
#16051=CARTESIAN_POINT('Ctrl Pts',(-0.105676786131388,-0.0744702911817869,
1.28757830688358));
#16052=CARTESIAN_POINT('Ctrl Pts',(-0.0175857351491984,-0.138091953858251,
1.29405531088083));
#16053=CARTESIAN_POINT('Ctrl Pts',(0.106487712804436,-0.089660542174548,
1.30199430051814));
#16054=CARTESIAN_POINT('Ctrl Pts',(0.133078957772855,0.0408489510387311,
1.30993329015544));
#16055=CARTESIAN_POINT('Ctrl Pts',(0.0378455373822902,0.133964029124136,
1.31787227979275));
#16056=CARTESIAN_POINT('Ctrl Pts',(-0.0855601048685178,0.105915403748908,
1.32541561258306));
#16057=CARTESIAN_POINT('Ctrl Pts',(-0.117590074669608,0.0331395035428114,
1.33031261549427));
#16058=CARTESIAN_POINT('Ctrl Pts',(-0.117871679003533,-9.01049542302501E-5,
1.33256328852638));
#16059=CARTESIAN_POINT('Ctrl Pts',(-0.117823716245033,-0.000102811805890825,
1.29243671147362));
#16060=CARTESIAN_POINT('Ctrl Pts',(-0.117892441435953,-0.00760726064997237,
1.29294445975461));
#16061=CARTESIAN_POINT('Ctrl Pts',(-0.113819337750002,-0.0541654333254181,
1.29609959740987));
#16062=CARTESIAN_POINT('Ctrl Pts',(-0.0518146499729274,-0.129225073214149,
1.30190212443939));
#16063=CARTESIAN_POINT('Ctrl Pts',(0.0805213734929343,-0.11357898534207,
1.30984429256217));
#16064=CARTESIAN_POINT('Ctrl Pts',(0.1390915465469,0.0061171215252809,1.31778646068495));
#16065=CARTESIAN_POINT('Ctrl Pts',(0.0702395735793815,0.120209316621791,
1.32572862880773));
#16066=CARTESIAN_POINT('Ctrl Pts',(-0.0629590648350173,0.124177428154433,
1.33367079693051));
#16067=CARTESIAN_POINT('Ctrl Pts',(-0.115917830154768,0.0471875384414626,
1.33924015781913));
#16068=CARTESIAN_POINT('Ctrl Pts',(-0.117945510062545,0.00411888419242175,
1.3421621293335));
#16069=CARTESIAN_POINT('Ctrl Pts',(-0.117917347702326,6.89762296073276E-5,
1.34243671147361));
#16070=CARTESIAN_POINT('Origin',(0.,0.,-0.0924367114736175));
#16071=CARTESIAN_POINT('',(-0.11774949833287,0.000107383800510985,1.23256328852638));
#16072=CARTESIAN_POINT('',(-0.117581795058195,-8.20683476789735E-6,1.24243671147361));
#16073=CARTESIAN_POINT('',(-0.117775,2.85464118895969E-14,-0.0924367114736175));
#16074=CARTESIAN_POINT('Ctrl Pts',(-0.11774949833287,0.000107383800510997,
1.23256328852638));
#16075=CARTESIAN_POINT('Ctrl Pts',(-0.1174869159147,-0.0291008736543001,
1.23453632015749));
#16076=CARTESIAN_POINT('Ctrl Pts',(-0.0917482398636095,-0.0978979247776974,
1.23915568166769));
#16077=CARTESIAN_POINT('Ctrl Pts',(0.0236422145726536,-0.137184880695923,
1.246421373057));
#16078=CARTESIAN_POINT('Ctrl Pts',(0.128082862902196,-0.0545291301253663,
1.2543603626943));
#16079=CARTESIAN_POINT('Ctrl Pts',(0.115272428336817,0.0780443019497631,
1.26229935233161));
#16080=CARTESIAN_POINT('Ctrl Pts',(-0.00306201423577413,0.139173524314926,
1.27023834196891));
#16081=CARTESIAN_POINT('Ctrl Pts',(-0.101358337705897,0.08278581645186,
1.27699298736717));
#16082=CARTESIAN_POINT('Ctrl Pts',(-0.117535345263889,0.02168343817453,
1.28110130288633));
#16083=CARTESIAN_POINT('Ctrl Pts',(-0.117590388001671,-3.33269891444124E-5,
1.28256328852638));
#16084=CARTESIAN_POINT('Ctrl Pts',(-0.117581795058195,-8.20683476789562E-6,
1.24243671147361));
#16085=CARTESIAN_POINT('Ctrl Pts',(-0.117593699448189,-0.0191748937105988,
1.24372679017572));
#16086=CARTESIAN_POINT('Ctrl Pts',(-0.104100832827715,-0.0776580224685839,
1.24766425825208));
#16087=CARTESIAN_POINT('Ctrl Pts',(-0.0120149744006178,-0.138706589206355,
1.25424911570271));
#16088=CARTESIAN_POINT('Ctrl Pts',(0.110059129405696,-0.0852693704304675,
1.26219128382548));
#16089=CARTESIAN_POINT('Ctrl Pts',(0.13130776387206,0.0462833517151888,
1.27013345194827));
#16090=CARTESIAN_POINT('Ctrl Pts',(0.0322649968732001,0.135435768819968,
1.27807562007105));
#16091=CARTESIAN_POINT('Ctrl Pts',(-0.0881142830049797,0.102747609761224,
1.28551003991283));
#16092=CARTESIAN_POINT('Ctrl Pts',(-0.117534109666069,0.0315207854174475,
1.29029707038035));
#16093=CARTESIAN_POINT('Ctrl Pts',(-0.117823716245033,-0.000102811805890825,
1.29243671147362));
#16094=CARTESIAN_POINT('Origin',(0.,0.,-0.0924367114736175));
#16095=CARTESIAN_POINT('',(-0.117957988745754,-3.12301727557783E-5,1.18256328852638));
#16096=CARTESIAN_POINT('',(-0.117793553451004,0.000106755881474893,1.19243671147362));
#16097=CARTESIAN_POINT('',(-0.117775,2.85464118895969E-14,-0.0924367114736175));
#16098=CARTESIAN_POINT('Ctrl Pts',(-0.117957988745754,-3.12301727557569E-5,
1.18256328852638));
#16099=CARTESIAN_POINT('Ctrl Pts',(-0.117964007145535,-0.00173159226684161,
1.18267867767044));
#16100=CARTESIAN_POINT('Ctrl Pts',(-0.117160216762375,-0.0424221720604921,
1.1854403966936));
#16101=CARTESIAN_POINT('Ctrl Pts',(-0.0703321751825429,-0.12013338809653,
1.19084844559586));
#16102=CARTESIAN_POINT('Ctrl Pts',(0.0627954496153871,-0.124239193932754,
1.19878743523316));
#16103=CARTESIAN_POINT('Ctrl Pts',(0.138438143943654,-0.0146125323915816,
1.20672642487047));
#16104=CARTESIAN_POINT('Ctrl Pts',(0.0873502052771435,0.108390901091839,
1.21466541450777));
#16105=CARTESIAN_POINT('Ctrl Pts',(-0.043700859820065,0.132169893139269,
1.22260440414508));
#16106=CARTESIAN_POINT('Ctrl Pts',(-0.112119660921406,0.0591163174148552,
1.22857036215128));
#16107=CARTESIAN_POINT('Ctrl Pts',(-0.117839104743291,0.0100747194789664,
1.23188999027838));
#16108=CARTESIAN_POINT('Ctrl Pts',(-0.11774949833287,0.000107383800510997,
1.23256328852638));
#16109=CARTESIAN_POINT('Ctrl Pts',(-0.117793553451004,0.000106755881474891,
1.19243671147362));
#16110=CARTESIAN_POINT('Ctrl Pts',(-0.117510050331475,-0.0305433296418112,
1.19450912059683));
#16111=CARTESIAN_POINT('Ctrl Pts',(-0.0896091397727994,-0.100804620014092,
1.19922891909429));
#16112=CARTESIAN_POINT('Ctrl Pts',(0.0288222657999454,-0.136209964735594,
1.20659610696603));
#16113=CARTESIAN_POINT('Ctrl Pts',(0.130092623711363,-0.0495962373069701,
1.21453827508881));
#16114=CARTESIAN_POINT('Ctrl Pts',(0.112184773380136,0.082452738709893,
1.22248044321158));
#16115=CARTESIAN_POINT('Ctrl Pts',(-0.00849585454694533,0.138966535376798,
1.23042261133437));
#16116=CARTESIAN_POINT('Ctrl Pts',(-0.103054997843392,0.079672038485689,
1.23707470075504));
#16117=CARTESIAN_POINT('Ctrl Pts',(-0.11756927027536,0.0201573447738481,
1.24107940080146));
#16118=CARTESIAN_POINT('Ctrl Pts',(-0.117581795058195,-8.20683476789562E-6,
1.24243671147361));
#16119=CARTESIAN_POINT('Origin',(0.,0.,-0.0924367114736175));
#16120=CARTESIAN_POINT('',(-0.117657565919426,-8.78585414499747E-5,1.13256328852638));
#16121=CARTESIAN_POINT('',(-0.117937823388479,-5.4172489969917E-5,1.14243671147362));
#16122=CARTESIAN_POINT('',(-0.117775,2.85464118895969E-14,-0.0924367114736175));
#16123=CARTESIAN_POINT('Ctrl Pts',(-0.117657565919426,-8.78585414499974E-5,
1.13256328852638));
#16124=CARTESIAN_POINT('Ctrl Pts',(-0.11775046973706,-0.0134980674796043,
1.13346736506249));
#16125=CARTESIAN_POINT('Ctrl Pts',(-0.109441032251172,-0.0660497484721492,
1.13701777147771));
#16126=CARTESIAN_POINT('Ctrl Pts',(-0.0320511128216771,-0.13546723577438,
1.14321450777202));
#16127=CARTESIAN_POINT('Ctrl Pts',(0.0964380908528195,-0.100390938007982,
1.15115349740933));
#16128=CARTESIAN_POINT('Ctrl Pts',(0.136644831685568,0.0265863832644056,
1.15909248704664));
#16129=CARTESIAN_POINT('Ctrl Pts',(0.0517625939920979,0.129225692742072,
1.16703147668394));
#16130=CARTESIAN_POINT('Ctrl Pts',(-0.0785823129332351,0.113795317289389,
1.17485507717719));
#16131=CARTESIAN_POINT('Ctrl Pts',(-0.117825981412732,0.0372644419932696,
1.18003234779134));
#16132=CARTESIAN_POINT('Ctrl Pts',(-0.117957988745754,-3.12301727557569E-5,
1.18256328852638));
#16133=CARTESIAN_POINT('Ctrl Pts',(-0.117937823388479,-5.41724899699178E-5,
1.14243671147362));
#16134=CARTESIAN_POINT('Ctrl Pts',(-0.117955293269658,-0.0031110520517566,
1.14264406164367));
#16135=CARTESIAN_POINT('Ctrl Pts',(-0.116460933142332,-0.0451799670343263,
1.14549880118799));
#16136=CARTESIAN_POINT('Ctrl Pts',(-0.0660858892268601,-0.122541963197144,
1.15100093010657));
#16137=CARTESIAN_POINT('Ctrl Pts',(0.0671705316110708,-0.121950798202395,
1.15894309822935));
#16138=CARTESIAN_POINT('Ctrl Pts',(0.138891844802359,-0.00964017357273747,
1.16688526635212));
#16139=CARTESIAN_POINT('Ctrl Pts',(0.0833739592533277,0.111501840422208,
1.17482743447491));
#16140=CARTESIAN_POINT('Ctrl Pts',(-0.0485230383040216,0.130496713571114,
1.18276960259768));
#16141=CARTESIAN_POINT('Ctrl Pts',(-0.113150295826959,0.0561813708375219,
1.18863936159726));
#16142=CARTESIAN_POINT('Ctrl Pts',(-0.117872210070015,0.00861047923971886,
1.19186173122257));
#16143=CARTESIAN_POINT('Ctrl Pts',(-0.117793553451004,0.000106755881474891,
1.19243671147362));
#16144=CARTESIAN_POINT('Origin',(0.,0.,-0.0924367114736175));
#16145=CARTESIAN_POINT('',(-0.117641451221435,8.0229283111194E-5,1.08256328852638));
#16146=CARTESIAN_POINT('',(-0.117630591849015,-7.42484764288953E-5,1.09243671147362));
#16147=CARTESIAN_POINT('',(-0.117775,2.85464118895969E-14,-0.0924367114736175));
#16148=CARTESIAN_POINT('Ctrl Pts',(-0.117641451221435,8.02292831111745E-5,
1.08256328852638));
#16149=CARTESIAN_POINT('Ctrl Pts',(-0.117483998834985,-0.0250372639622414,
1.08425605245455));
#16150=CARTESIAN_POINT('Ctrl Pts',(-0.0972946570053161,-0.0896524615425008,
1.08859514626182));
#16151=CARTESIAN_POINT('Ctrl Pts',(0.00904258428980543,-0.13891320121148,
1.09558056994819));
#16152=CARTESIAN_POINT('Ctrl Pts',(0.121617839487272,-0.067732908692211,
1.1035195595855));
#16153=CARTESIAN_POINT('Ctrl Pts',(0.122860297649024,0.0654522196953821,
1.1114585492228));
#16154=CARTESIAN_POINT('Ctrl Pts',(0.0116325734791967,0.138720326685422,
1.11939753886011));
#16155=CARTESIAN_POINT('Ctrl Pts',(-0.096364912740844,0.0911171059582243,
1.1264324519613));
#16156=CARTESIAN_POINT('Ctrl Pts',(-0.117478530206868,0.0257550656131636,
1.13082103518339));
#16157=CARTESIAN_POINT('Ctrl Pts',(-0.117657565919426,-8.78585414499974E-5,
1.13256328852638));
#16158=CARTESIAN_POINT('Ctrl Pts',(-0.117630591849015,-7.42484764288814E-5,
1.09243671147362));
#16159=CARTESIAN_POINT('Ctrl Pts',(-0.117715241483118,-0.0147626739157663,
1.09342639206478));
#16160=CARTESIAN_POINT('Ctrl Pts',(-0.108350501834675,-0.0686384992808382,
1.0970634620302));
#16161=CARTESIAN_POINT('Ctrl Pts',(-0.0276126195379174,-0.136460326620484,
1.10334792136989));
#16162=CARTESIAN_POINT('Ctrl Pts',(0.0997182217817603,-0.0971604536002107,
1.11129008949267));
#16163=CARTESIAN_POINT('Ctrl Pts',(0.135696927507188,0.0311483765905046,
1.11923225761545));
#16164=CARTESIAN_POINT('Ctrl Pts',(0.0473633069609982,0.130922093830007,
1.12717442573822));
#16165=CARTESIAN_POINT('Ctrl Pts',(-0.0809210029008042,0.111284164335459,
1.13490924369095));
#16166=CARTESIAN_POINT('Ctrl Pts',(-0.117732242679493,0.0359183370635313,
1.13999667226941));
#16167=CARTESIAN_POINT('Ctrl Pts',(-0.117937823388479,-5.41724899699178E-5,
1.14243671147362));
#16168=CARTESIAN_POINT('Origin',(0.,0.,-0.0924367114736175));
#16169=CARTESIAN_POINT('',(-0.117948158721073,4.38502512853227E-5,1.03256328852638));
#16170=CARTESIAN_POINT('',(-0.117667547954054,9.20194976846214E-5,1.04243671147362));
#16171=CARTESIAN_POINT('',(-0.117775,2.85464118895969E-14,-0.0924367114736175));
#16172=CARTESIAN_POINT('Ctrl Pts',(-0.117948158721073,4.38502512853157E-5,
1.03256328852638));
#16173=CARTESIAN_POINT('Ctrl Pts',(-0.117773439871091,-0.0365306738650768,
1.03504473984661));
#16174=CARTESIAN_POINT('Ctrl Pts',(-0.0798690478914953,-0.112422454385097,
1.04017252104593));
#16175=CARTESIAN_POINT('Ctrl Pts',(0.0493427524230464,-0.130168884856471,
1.04794663212436));
#16176=CARTESIAN_POINT('Ctrl Pts',(0.136125055048066,-0.0291310004912345,
1.05588562176166));
#16177=CARTESIAN_POINT('Ctrl Pts',(0.0982941990358779,0.0985743183458784,
1.06382461139897));
#16178=CARTESIAN_POINT('Ctrl Pts',(-0.0295182596522469,0.136041604476578,
1.07176360103627));
#16179=CARTESIAN_POINT('Ctrl Pts',(-0.108818061611988,0.067537217334308,
1.07800982674541));
#16180=CARTESIAN_POINT('Ctrl Pts',(-0.11773014713001,0.0142293884972668,
1.08160972257545));
#16181=CARTESIAN_POINT('Ctrl Pts',(-0.117641451221435,8.02292831111745E-5,
1.08256328852638));
#16182=CARTESIAN_POINT('Ctrl Pts',(-0.117667547954054,9.20194976846197E-5,
1.04243671147362));
#16183=CARTESIAN_POINT('Ctrl Pts',(-0.117475882803567,-0.0261866690710452,
1.04420872248589));
#16184=CARTESIAN_POINT('Ctrl Pts',(-0.0957916308421219,-0.0920126959480487,
1.04862812287242));
#16185=CARTESIAN_POINT('Ctrl Pts',(0.0132451643780021,-0.13859452774087,
1.05569491263321));
#16186=CARTESIAN_POINT('Ctrl Pts',(0.123654649330263,-0.0639797248987874,
1.06363708075599));
#16187=CARTESIAN_POINT('Ctrl Pts',(0.120783771971213,0.0692470788374567,
1.07157924887876));
#16188=CARTESIAN_POINT('Ctrl Pts',(0.00726255089817806,0.139036444335888,
1.07952141700155));
#16189=CARTESIAN_POINT('Ctrl Pts',(-0.0979368667310299,0.0886295245336828,
1.08647390453316));
#16190=CARTESIAN_POINT('Ctrl Pts',(-0.117488804242801,0.0245287720112504,
1.09077900269052));
#16191=CARTESIAN_POINT('Ctrl Pts',(-0.117630591849015,-7.42484764288814E-5,
1.09243671147362));
#16192=CARTESIAN_POINT('Origin',(0.,0.,-0.0924367114736175));
#16193=CARTESIAN_POINT('',(-0.117771476475648,-0.000107683352847938,0.982563288526384));
#16194=CARTESIAN_POINT('',(-0.11796176292438,2.53781033017321E-5,0.992436711473616));
#16195=CARTESIAN_POINT('',(-0.117775,2.85464118895969E-14,-0.0924367114736175));
#16196=CARTESIAN_POINT('Ctrl Pts',(-0.117771476475648,-0.000107683352847945,
0.982563288526384));
#16197=CARTESIAN_POINT('Ctrl Pts',(-0.117856103358663,-0.00933799346614349,
0.983187097359559));
#16198=CARTESIAN_POINT('Ctrl Pts',(-0.112646870919438,-0.057630810124202,
0.986457236071836));
#16199=CARTESIAN_POINT('Ctrl Pts',(-0.0461590140787468,-0.131331607851033,
0.992373704663214));
#16200=CARTESIAN_POINT('Ctrl Pts',(0.0853128637208732,-0.110001641284132,
1.00031269430052));
#16201=CARTESIAN_POINT('Ctrl Pts',(0.138686661656432,0.0120272889735618,
1.00825168393783));
#16202=CARTESIAN_POINT('Ctrl Pts',(0.0651023256631918,0.123046060459907,
1.01619067357513));
#16203=CARTESIAN_POINT('Ctrl Pts',(-0.0680787277209358,0.121424596492465,
1.02412966321244));
#16204=CARTESIAN_POINT('Ctrl Pts',(-0.116790117880403,0.0438975063746073,
1.02958720152952));
#16205=CARTESIAN_POINT('Ctrl Pts',(-0.11795976781127,0.00247402277930658,
1.0323984099675));
#16206=CARTESIAN_POINT('Ctrl Pts',(-0.117948158721073,4.38502512853157E-5,
1.03256328852638));
#16207=CARTESIAN_POINT('Ctrl Pts',(-0.11796176292438,2.53781033017319E-5,
0.992436711473616));
#16208=CARTESIAN_POINT('Ctrl Pts',(-0.117851518882229,-0.0376119105440478,
0.994991052906992));
#16209=CARTESIAN_POINT('Ctrl Pts',(-0.077958511321084,-0.114458475672252,
1.00019278371463));
#16210=CARTESIAN_POINT('Ctrl Pts',(0.0529591494285269,-0.128760265574912,
1.00804190389653));
#16211=CARTESIAN_POINT('Ctrl Pts',(0.136912761112491,-0.0252739657289669,
1.0159840720193));
#16212=CARTESIAN_POINT('Ctrl Pts',(0.0954402180350474,0.101365883217864,
1.02392624014209));
#16213=CARTESIAN_POINT('Ctrl Pts',(-0.0334653697086341,0.135144169424284,
1.03186840826486));
#16214=CARTESIAN_POINT('Ctrl Pts',(-0.109792739119276,0.0652029671457737,
1.03803856537538));
#16215=CARTESIAN_POINT('Ctrl Pts',(-0.117762231070763,0.0130737646421874,
1.04156133311163));
#16216=CARTESIAN_POINT('Ctrl Pts',(-0.117667547954054,9.20194976846197E-5,
1.04243671147362));
#16217=CARTESIAN_POINT('Origin',(0.,0.,-0.0924367114736175));
#16218=CARTESIAN_POINT('',(-0.117585265278523,2.16484251076657E-5,0.932563288526384));
#16219=CARTESIAN_POINT('',(-0.117742563953077,-0.000107211314308964,0.942436711473616));
#16220=CARTESIAN_POINT('',(-0.117775,2.85464118895969E-14,-0.0924367114736175));
#16221=CARTESIAN_POINT('Ctrl Pts',(-0.117585265278523,2.16484251076635E-5,
0.932563288526384));
#16222=CARTESIAN_POINT('Ctrl Pts',(-0.117550805757046,-0.0209622679161363,
0.933975784751614));
#16223=CARTESIAN_POINT('Ctrl Pts',(-0.102172791552808,-0.0813069697478888,
0.938034610855947));
#16224=CARTESIAN_POINT('Ctrl Pts',(-0.00565790085648466,-0.139092177922979,
0.944739766839381));
#16225=CARTESIAN_POINT('Ctrl Pts',(0.113796373024222,-0.0801812402497705,
0.952678756476687));
#16226=CARTESIAN_POINT('Ctrl Pts',(0.129077866376032,0.0521301276928276,
0.960617746113992));
#16227=CARTESIAN_POINT('Ctrl Pts',(0.026197419344502,0.13671993644362,0.968556735751298));
#16228=CARTESIAN_POINT('Ctrl Pts',(-0.0906967139502387,0.0993396518733501,
0.975871916555428));
#16229=CARTESIAN_POINT('Ctrl Pts',(-0.117497098103867,0.02981894716558,
0.980540767480457));
#16230=CARTESIAN_POINT('Ctrl Pts',(-0.117771476475648,-0.000107683352847945,
0.982563288526384));
#16231=CARTESIAN_POINT('Ctrl Pts',(-0.117742563953077,-0.000107211314308957,
0.942436711473616));
#16232=CARTESIAN_POINT('Ctrl Pts',(-0.117833632602859,-0.0103126986533654,
0.943125993953839));
#16233=CARTESIAN_POINT('Ctrl Pts',(-0.111944766202914,-0.0596118697348184,
0.946462665808322));
#16234=CARTESIAN_POINT('Ctrl Pts',(-0.0428565117498991,-0.132465832952297,
0.952446727037066));
#16235=CARTESIAN_POINT('Ctrl Pts',(0.0880997963686447,-0.107806787258123,
0.960388895159846));
#16236=CARTESIAN_POINT('Ctrl Pts',(0.138347640177547,0.0156143509765511,
0.968331063282625));
#16237=CARTESIAN_POINT('Ctrl Pts',(0.061854832590724,0.124731139593481,
0.976273231405407));
#16238=CARTESIAN_POINT('Ctrl Pts',(-0.0713033562375951,0.119581390225944,
0.984215399528185));
#16239=CARTESIAN_POINT('Ctrl Pts',(-0.117322772537986,0.0417718924351975,
0.989603226217589));
#16240=CARTESIAN_POINT('Ctrl Pts',(-0.11796577882491,0.00139640554830399,
0.992343663532733));
#16241=CARTESIAN_POINT('Ctrl Pts',(-0.11796176292438,2.53781033017319E-5,
0.992436711473616));
#16242=CARTESIAN_POINT('Origin',(0.,0.,-0.0924367114736175));
#16243=CARTESIAN_POINT('',(-0.117850913371472,9.6525574830472E-5,0.882563288526384));
#16244=CARTESIAN_POINT('',(-0.117591231449503,3.54948526558943E-5,0.892436711473616));
#16245=CARTESIAN_POINT('',(-0.117775,2.85464118895969E-14,-0.0924367114736175));
#16246=CARTESIAN_POINT('Ctrl Pts',(-0.117850913371472,9.65255748304767E-5,
0.882563288526384));
#16247=CARTESIAN_POINT('Ctrl Pts',(-0.117563006813672,-0.0324172738354332,
0.884764472143669));
#16248=CARTESIAN_POINT('Ctrl Pts',(-0.0867151192651892,-0.104499852648429,
0.889611985640057));
#16249=CARTESIAN_POINT('Ctrl Pts',(0.0353397195745277,-0.134646760160997,
0.897105829015547));
#16250=CARTESIAN_POINT('Ctrl Pts',(0.132293719443212,-0.0433245611326863,
0.905044818652852));
#16251=CARTESIAN_POINT('Ctrl Pts',(0.108141885842356,0.0876583043865096,
0.912983808290157));
#16252=CARTESIAN_POINT('Ctrl Pts',(-0.0150064327997127,0.138395999855801,
0.920922797927463));
#16253=CARTESIAN_POINT('Ctrl Pts',(-0.104951114476159,0.0759553573435841,
0.927449291339539));
#16254=CARTESIAN_POINT('Ctrl Pts',(-0.117615366114572,0.01835136974357,
0.931329454872513));
#16255=CARTESIAN_POINT('Ctrl Pts',(-0.117585265278523,2.16484251076635E-5,
0.932563288526384));
#16256=CARTESIAN_POINT('Ctrl Pts',(-0.117591231449503,3.54948526559117E-5,
0.892436711473616));
#16257=CARTESIAN_POINT('Ctrl Pts',(-0.117532234588281,-0.0218238662162972,
0.893908324374946));
#16258=CARTESIAN_POINT('Ctrl Pts',(-0.101194437785642,-0.0830895288483654,
0.898027326650536));
#16259=CARTESIAN_POINT('Ctrl Pts',(-0.00250162451743248,-0.139203517821528,
0.904793718300386));
#16260=CARTESIAN_POINT('Ctrl Pts',(0.115632500949424,-0.0775435504945224,
0.912735886423165));
#16261=CARTESIAN_POINT('Ctrl Pts',(0.127835376168433,0.0551542754370876,
0.920678054545947));
#16262=CARTESIAN_POINT('Ctrl Pts',(0.0229279137899797,0.137325118854324,
0.928620222668725));
#16263=CARTESIAN_POINT('Ctrl Pts',(-0.0920562790907298,0.0974788594069619,
0.935873108311283));
#16264=CARTESIAN_POINT('Ctrl Pts',(-0.117483857027998,0.0288844367965532,
0.94047860457958));
#16265=CARTESIAN_POINT('Ctrl Pts',(-0.117742563953077,-0.000107211314308957,
0.942436711473616));
#16266=CARTESIAN_POINT('Origin',(0.,0.,-0.0924367114736175));
#16267=CARTESIAN_POINT('',(-0.11789232318732,-8.18790992476613E-5,0.832563288526384));
#16268=CARTESIAN_POINT('',(-0.117872825429845,8.99519344067963E-5,0.842436711473616));
#16269=CARTESIAN_POINT('',(-0.117775,2.85464118895969E-14,-0.0924367114736175));
#16270=CARTESIAN_POINT('Ctrl Pts',(-0.11789232318732,-8.18790992476734E-5,
0.832563288526384));
#16271=CARTESIAN_POINT('Ctrl Pts',(-0.117932494517479,-0.00515170743829337,
0.832906829656623));
#16272=CARTESIAN_POINT('Ctrl Pts',(-0.115332713682068,-0.0492334187378749,
0.835896700665964));
#16273=CARTESIAN_POINT('Ctrl Pts',(-0.059752088941783,-0.125731196083361,
0.841532901554406));
#16274=CARTESIAN_POINT('Ctrl Pts',(0.0732361146625898,-0.118385460722959,
0.849471891191712));
#16275=CARTESIAN_POINT('Ctrl Pts',(0.139181674492094,-0.00266594955618734,
0.857410880829018));
#16276=CARTESIAN_POINT('Ctrl Pts',(0.077715950067195,0.115494055719818,
0.865349870466323));
#16277=CARTESIAN_POINT('Ctrl Pts',(-0.0548934004223171,0.127927168308903,
0.87328886010363));
#16278=CARTESIAN_POINT('Ctrl Pts',(-0.114416768398411,0.0522742940766184,
0.879026666123649));
#16279=CARTESIAN_POINT('Ctrl Pts',(-0.117909136832228,0.0066718045071592,
0.882118142264567));
#16280=CARTESIAN_POINT('Ctrl Pts',(-0.117850913371472,9.65255748304767E-5,
0.882563288526384));
#16281=CARTESIAN_POINT('Ctrl Pts',(-0.117872825429845,8.99519344067998E-5,
0.842436711473616));
#16282=CARTESIAN_POINT('Ctrl Pts',(-0.117591169542271,-0.0331870933343037,
0.844690654796053));
#16283=CARTESIAN_POINT('Ctrl Pts',(-0.0854771005934613,-0.106025606004136,
0.84959198749275));
#16284=CARTESIAN_POINT('Ctrl Pts',(0.0380692928980519,-0.133920149482284,
0.857140709563706));
#16285=CARTESIAN_POINT('Ctrl Pts',(0.133179650076608,-0.0405839661022353,
0.865082877686486));
#16286=CARTESIAN_POINT('Ctrl Pts',(0.106283765719693,0.0899312995767124,
0.873025045809266));
#16287=CARTESIAN_POINT('Ctrl Pts',(-0.0179789669825735,0.138060255849953,
0.880967213932046));
#16288=CARTESIAN_POINT('Ctrl Pts',(-0.105798194743126,0.0742290978659706,
0.887437769153496));
#16289=CARTESIAN_POINT('Ctrl Pts',(-0.117638368248411,0.0175004969839459,
0.891260935000686));
#16290=CARTESIAN_POINT('Ctrl Pts',(-0.117591231449503,3.54948526559117E-5,
0.892436711473616));
#16291=CARTESIAN_POINT('Origin',(0.,0.,-0.0924367114736175));
#16292=CARTESIAN_POINT('',(-0.117598114366551,-4.51832715892789E-5,0.782563288526384));
#16293=CARTESIAN_POINT('',(-0.117874685330111,-8.92836445515327E-5,0.792436711473617));
#16294=CARTESIAN_POINT('',(-0.117775,2.85464118895969E-14,-0.0924367114736175));
#16295=CARTESIAN_POINT('Ctrl Pts',(-0.117598114366551,-4.518327158929E-5,
0.782563288526384));
#16296=CARTESIAN_POINT('Ctrl Pts',(-0.117656123976761,-0.0168608793038394,
0.783695517048678));
#16297=CARTESIAN_POINT('Ctrl Pts',(-0.106420815930739,-0.0729055463807818,
0.787474075450074));
#16298=CARTESIAN_POINT('Ctrl Pts',(-0.0202952816069424,-0.137719814645367,
0.793898963730571));
#16299=CARTESIAN_POINT('Ctrl Pts',(0.104705698854998,-0.0917352845351548,
0.801837953367879));
#16300=CARTESIAN_POINT('Ctrl Pts',(0.133855787965376,0.0382266115373486,
0.809776943005182));
#16301=CARTESIAN_POINT('Ctrl Pts',(0.0404700769297216,0.133194664588195,
0.81771593264249));
#16302=CARTESIAN_POINT('Ctrl Pts',(-0.0843190215395119,0.107398870964955,
0.825311381149555));
#16303=CARTESIAN_POINT('Ctrl Pts',(-0.117623050954756,0.0339016606582783,
0.830260499777521));
#16304=CARTESIAN_POINT('Ctrl Pts',(-0.11789232318732,-8.18790992476734E-5,
0.832563288526384));
#16305=CARTESIAN_POINT('Ctrl Pts',(-0.117874685330111,-8.9283644551537E-5,
0.792436711473617));
#16306=CARTESIAN_POINT('Ctrl Pts',(-0.11792303416021,-0.00583050672374999,
0.7928255958429));
#16307=CARTESIAN_POINT('Ctrl Pts',(-0.114931453360353,-0.0506053896743902,
0.795861869586443));
#16308=CARTESIAN_POINT('Ctrl Pts',(-0.0575513573065257,-0.126774282767806,
0.801545532704245));
#16309=CARTESIAN_POINT('Ctrl Pts',(0.0753527000357912,-0.117071978271622,
0.809487700827026));
#16310=CARTESIAN_POINT('Ctrl Pts',(0.139225942868322,-0.000119714417332432,
0.817429868949805));
#16311=CARTESIAN_POINT('Ctrl Pts',(0.0755539188089132,0.116942220141962,
0.825372037072586));
#16312=CARTESIAN_POINT('Ctrl Pts',(-0.0573332568284509,0.12687306712048,
0.833314205195366));
#16313=CARTESIAN_POINT('Ctrl Pts',(-0.114890414736801,0.0507419104293215,
0.839002429995709));
#16314=CARTESIAN_POINT('Ctrl Pts',(-0.117921990994851,0.00589875908008548,
0.842043265421793));
#16315=CARTESIAN_POINT('Ctrl Pts',(-0.117872825429845,8.99519344067998E-5,
0.842436711473616));
#16316=CARTESIAN_POINT('Origin',(0.,0.,-0.0924367114736175));
#16317=CARTESIAN_POINT('',(-0.11772691567491,0.000105512987197037,0.732563288526384));
#16318=CARTESIAN_POINT('',(-0.117591850253004,-3.65476421498312E-5,0.742436711473616));
#16319=CARTESIAN_POINT('',(-0.117775,2.85464118895969E-14,-0.0924367114736175));
#16320=CARTESIAN_POINT('Ctrl Pts',(-0.11772691567491,0.000105512987197042,
0.732563288526384));
#16321=CARTESIAN_POINT('Ctrl Pts',(-0.117479624464894,-0.0283451130369189,
0.734484204440733));
#16322=CARTESIAN_POINT('Ctrl Pts',(-0.0928318426870313,-0.096374559506161,
0.739051450234184));
#16323=CARTESIAN_POINT('Ctrl Pts',(0.0209425314183671,-0.137622876656644,
0.746265025906738));
#16324=CARTESIAN_POINT('Ctrl Pts',(0.126986869252672,-0.0570349089493802,
0.754204015544043));
#16325=CARTESIAN_POINT('Ctrl Pts',(0.11678343126468,0.0757646090434518,
0.762143005181349));
#16326=CARTESIAN_POINT('Ctrl Pts',(-0.000327234354877375,0.139206819944772,
0.770081994818654));
#16327=CARTESIAN_POINT('Ctrl Pts',(-0.100479183608201,0.0843410365921374,
0.776888755933667));
#16328=CARTESIAN_POINT('Ctrl Pts',(-0.117520539541507,0.0224420334666934,
0.781049187169576));
#16329=CARTESIAN_POINT('Ctrl Pts',(-0.117598114366551,-4.518327158929E-5,
0.782563288526384));
#16330=CARTESIAN_POINT('Ctrl Pts',(-0.117591850253004,-3.65476421498364E-5,
0.742436711473616));
#16331=CARTESIAN_POINT('Ctrl Pts',(-0.117640211257931,-0.0174335619022046,
0.743607926264006));
#16332=CARTESIAN_POINT('Ctrl Pts',(-0.105863856762799,-0.0740921523660566,
0.747426530428656));
#16333=CARTESIAN_POINT('Ctrl Pts',(-0.0182163644075178,-0.138029133036789,
0.753892523967566));
#16334=CARTESIAN_POINT('Ctrl Pts',(0.106128952536144,-0.0901139441634624,
0.761834692090347));
#16335=CARTESIAN_POINT('Ctrl Pts',(0.133249245915149,0.0403548753208232,
0.769776860213125));
#16336=CARTESIAN_POINT('Ctrl Pts',(0.0382995408207276,0.133854483197375,
0.777719028335907));
#16337=CARTESIAN_POINT('Ctrl Pts',(-0.0853693283863186,0.106155717082476,
0.785272312089402));
#16338=CARTESIAN_POINT('Ctrl Pts',(-0.117593892160246,0.0332537408718532,
0.79017820646864));
#16339=CARTESIAN_POINT('Ctrl Pts',(-0.117874685330111,-8.9283644551537E-5,
0.792436711473617));
#16340=CARTESIAN_POINT('Origin',(0.,0.,-0.0924367114736175));
#16341=CARTESIAN_POINT('',(-0.117964947617991,-1.73329198795185E-5,0.682563288526384));
#16342=CARTESIAN_POINT('',(-0.117740574064672,0.000107068518266168,0.692436711473616));
#16343=CARTESIAN_POINT('',(-0.117775,2.85464118895969E-14,-0.0924367114736175));
#16344=CARTESIAN_POINT('Ctrl Pts',(-0.117964947617991,-1.73329198795367E-5,
0.682563288526384));
#16345=CARTESIAN_POINT('Ctrl Pts',(-0.117966864156947,-0.000949576032666658,
0.682626561953687));
#16346=CARTESIAN_POINT('Ctrl Pts',(-0.117534558560489,-0.0408698671952461,
0.685336165260092));
#16347=CARTESIAN_POINT('Ctrl Pts',(-0.0726787294560835,-0.118728463672822,
0.690692098445597));
#16348=CARTESIAN_POINT('Ctrl Pts',(0.0603425395611779,-0.125448888878168,
0.698631088082904));
#16349=CARTESIAN_POINT('Ctrl Pts',(0.138124349154501,-0.0173294538893964,
0.706570077720209));
#16350=CARTESIAN_POINT('Ctrl Pts',(0.0894627833767505,0.106653908470079,
0.714509067357515));
#16351=CARTESIAN_POINT('Ctrl Pts',(-0.0410958292974484,0.133002927094911,
0.72244805699482));
#16352=CARTESIAN_POINT('Ctrl Pts',(-0.111546724107196,0.0606813038481789,
0.728466130717777));
#16353=CARTESIAN_POINT('Ctrl Pts',(-0.117820302634623,0.0108495967181263,
0.731837874561632));
#16354=CARTESIAN_POINT('Ctrl Pts',(-0.11772691567491,0.000105512987197042,
0.732563288526384));
#16355=CARTESIAN_POINT('Ctrl Pts',(-0.117740574064672,0.000107068518266165,
0.692436711473616));
#16356=CARTESIAN_POINT('Ctrl Pts',(-0.117483171888848,-0.0288182833237499,
0.694390256685113));
#16357=CARTESIAN_POINT('Ctrl Pts',(-0.0921515028359353,-0.0973455904149804,
0.698991191270869));
#16358=CARTESIAN_POINT('Ctrl Pts',(0.022691720100341,-0.137364345221032,
0.706239515230886));
#16359=CARTESIAN_POINT('Ctrl Pts',(0.127740337615313,-0.0553740340325759,
0.714181683353665));
#16360=CARTESIAN_POINT('Ctrl Pts',(0.115765682611161,0.077344581120379,
0.722123851476446));
#16361=CARTESIAN_POINT('Ctrl Pts',(-0.00226223072526165,0.139207614056346,
0.730066019599226));
#16362=CARTESIAN_POINT('Ctrl Pts',(-0.101117998472899,0.083225715609228,
0.736836972931616));
#16363=CARTESIAN_POINT('Ctrl Pts',(-0.117530897055598,0.0218902846491045,
0.740960536889746));
#16364=CARTESIAN_POINT('Ctrl Pts',(-0.117591850253004,-3.65476421498364E-5,
0.742436711473616));
#16365=CARTESIAN_POINT('Origin',(0.,0.,-0.0924367114736175));
#16366=CARTESIAN_POINT('',(-0.117676160015555,-9.46906955630148E-5,0.632563288526383));
#16367=CARTESIAN_POINT('',(-0.117962383120995,-2.41598447144192E-5,0.642436711473616));
#16368=CARTESIAN_POINT('',(-0.117775,2.85464118895969E-14,-0.0924367114736175));
#16369=CARTESIAN_POINT('Ctrl Pts',(-0.117676160015555,-9.46906955630045E-5,
0.632563288526383));
#16370=CARTESIAN_POINT('Ctrl Pts',(-0.117771520970562,-0.0127268345011372,
0.633415249345741));
#16371=CARTESIAN_POINT('Ctrl Pts',(-0.110078248258936,-0.064483421762156,
0.636913540044201));
#16372=CARTESIAN_POINT('Ctrl Pts',(-0.0347063025259737,-0.134811417789573,
0.643058160621763));
#16373=CARTESIAN_POINT('Ctrl Pts',(0.0944472082050275,-0.102266175560326,
0.65099715025907));
#16374=CARTESIAN_POINT('Ctrl Pts',(0.137140772714236,0.0238967416356601,
0.658936139896373));
#16375=CARTESIAN_POINT('Ctrl Pts',(0.054291358674537,0.128183829614862,
0.666875129533682));
#16376=CARTESIAN_POINT('Ctrl Pts',(-0.0772016597727435,0.11523146575827,
0.674750845743682));
#16377=CARTESIAN_POINT('Ctrl Pts',(-0.117886707375211,0.0380402955314478,
0.679980232074585));
#16378=CARTESIAN_POINT('Ctrl Pts',(-0.117964947617991,-1.73329198795367E-5,
0.682563288526384));
#16379=CARTESIAN_POINT('Ctrl Pts',(-0.117962383120995,-2.41598447144253E-5,
0.642436711473616));
#16380=CARTESIAN_POINT('Ctrl Pts',(-0.117966033213387,-0.0013279541977536,
0.642525197731959));
#16381=CARTESIAN_POINT('Ctrl Pts',(-0.117355585052125,-0.0416360146359673,
0.645261073364563));
#16382=CARTESIAN_POINT('Ctrl Pts',(-0.0715088964667609,-0.119458592094588,
0.650644338371427));
#16383=CARTESIAN_POINT('Ctrl Pts',(0.0616402393688536,-0.124837327709565,
0.658586506494205));
#16384=CARTESIAN_POINT('Ctrl Pts',(0.138320583400205,-0.0158522461166236,
0.666528674616987));
#16385=CARTESIAN_POINT('Ctrl Pts',(0.0882850628235238,0.107655121482266,
0.674470842739765));
#16386=CARTESIAN_POINT('Ctrl Pts',(-0.0426286451686149,0.132539337972556,
0.682413010862546));
#16387=CARTESIAN_POINT('Ctrl Pts',(-0.111894847147975,0.059748848130285,
0.68840163377383));
#16388=CARTESIAN_POINT('Ctrl Pts',(-0.117831996057943,0.0103805377030848,
0.691742867310853));
#16389=CARTESIAN_POINT('Ctrl Pts',(-0.117740574064672,0.000107068518266165,
0.692436711473616));
#16390=CARTESIAN_POINT('Origin',(0.,0.,-0.0924367114736175));
#16391=CARTESIAN_POINT('',(-0.117626285855324,7.11112359239178E-5,0.582563288526384));
#16392=CARTESIAN_POINT('',(-0.11766919235599,-9.26074537421634E-5,0.592436711473616));
#16393=CARTESIAN_POINT('',(-0.117775,2.85464118895969E-14,-0.0924367114736175));
#16394=CARTESIAN_POINT('Ctrl Pts',(-0.117626285855324,7.11112359239024E-5,
0.582563288526383));
#16395=CARTESIAN_POINT('Ctrl Pts',(-0.117492102008102,-0.0242809575267813,
0.584203936737797));
#16396=CARTESIAN_POINT('Ctrl Pts',(-0.0982512120079041,-0.0881067492982899,
0.588490914828312));
#16397=CARTESIAN_POINT('Ctrl Pts',(0.00631176444456456,-0.139064040754811,
0.595424222797929));
#16398=CARTESIAN_POINT('Ctrl Pts',(0.120263693490807,-0.0701091280034811,
0.603363212435234));
#16399=CARTESIAN_POINT('Ctrl Pts',(0.124122453355413,0.0630258865426945,
0.611302202072541));
#16400=CARTESIAN_POINT('Ctrl Pts',(0.0143556138404206,0.138465021405133,
0.619241191709845));
#16401=CARTESIAN_POINT('Ctrl Pts',(-0.0953630726970595,0.0926558297308384,
0.626328220527794));
#16402=CARTESIAN_POINT('Ctrl Pts',(-0.117475314221613,0.0265106736450616,
0.630768919466639));
#16403=CARTESIAN_POINT('Ctrl Pts',(-0.117676160015555,-9.46906955630045E-5,
0.632563288526383));
#16404=CARTESIAN_POINT('Ctrl Pts',(-0.11766919235599,-9.26074537421669E-5,
0.592436711473616));
#16405=CARTESIAN_POINT('Ctrl Pts',(-0.117764072896019,-0.0130062487266101,
0.593307528153066));
#16406=CARTESIAN_POINT('Ctrl Pts',(-0.109848366281979,-0.0650658641993071,
0.596825734206776));
#16407=CARTESIAN_POINT('Ctrl Pts',(-0.0336977294021144,-0.135086418755761,
0.602991329634746));
#16408=CARTESIAN_POINT('Ctrl Pts',(0.0952657566843092,-0.101529863106778,
0.610933497757526));
#16409=CARTESIAN_POINT('Ctrl Pts',(0.136956022624868,0.025038477707157,
0.618875665880307));
#16410=CARTESIAN_POINT('Ctrl Pts',(0.0531805018142573,0.128669000640787,
0.626817834003085));
#16411=CARTESIAN_POINT('Ctrl Pts',(-0.0778376600742765,0.114584191752874,
0.634671515867523));
#16412=CARTESIAN_POINT('Ctrl Pts',(-0.117856827377429,0.0376798124439797,
0.639877808357699));
#16413=CARTESIAN_POINT('Ctrl Pts',(-0.117962383120995,-2.41598447144253E-5,
0.642436711473616));
#16414=CARTESIAN_POINT('Origin',(0.,0.,-0.0924367114736175));
#16415=CARTESIAN_POINT('',(-0.117934829819181,5.63106208242181E-5,0.532563288526383));
#16416=CARTESIAN_POINT('',(-0.117629301205424,7.34277634442948E-5,0.542436711473615));
#16417=CARTESIAN_POINT('',(-0.117775,2.85464118895969E-14,-0.0924367114736175));
#16418=CARTESIAN_POINT('Ctrl Pts',(-0.117934829819181,5.63106208242166E-5,
0.532563288526383));
#16419=CARTESIAN_POINT('Ctrl Pts',(-0.117723349859012,-0.0357608023914865,
0.534992624129852));
#16420=CARTESIAN_POINT('Ctrl Pts',(-0.0811985738067347,-0.110967619805887,
0.540068289612422));
#16421=CARTESIAN_POINT('Ctrl Pts',(0.0467759446245483,-0.131113145053959,
0.547790284974095));
#16422=CARTESIAN_POINT('Ctrl Pts',(0.135526478334676,-0.031799677225719,
0.555729274611401));
#16423=CARTESIAN_POINT('Ctrl Pts',(0.100211809365564,0.0966242157284558,
0.563668264248707));
#16424=CARTESIAN_POINT('Ctrl Pts',(-0.0268399031138932,0.136595261273209,
0.571607253886012));
#16425=CARTESIAN_POINT('Ctrl Pts',(-0.108142973925314,0.0691035501437442,
0.577905595311905));
#16426=CARTESIAN_POINT('Ctrl Pts',(-0.117708537635025,0.0149983997031143,
0.581557606858695));
#16427=CARTESIAN_POINT('Ctrl Pts',(-0.117626285855324,7.11112359239024E-5,
0.582563288526383));
#16428=CARTESIAN_POINT('Ctrl Pts',(-0.117629301205424,7.34277634442983E-5,
0.542436711473615));
#16429=CARTESIAN_POINT('Ctrl Pts',(-0.11748956090956,-0.0244625652698295,
0.544089858574172));
#16430=CARTESIAN_POINT('Ctrl Pts',(-0.0980201725405651,-0.0884941619373469,
0.548390395048989));
#16431=CARTESIAN_POINT('Ctrl Pts',(0.00702343738442799,-0.139048728244533,
0.555338320898066));
#16432=CARTESIAN_POINT('Ctrl Pts',(0.12066450826877,-0.0694546898587181,
0.563280489020846));
#16433=CARTESIAN_POINT('Ctrl Pts',(0.123764493242992,0.063766979789076,
0.571222657143626));
#16434=CARTESIAN_POINT('Ctrl Pts',(0.0134834875971477,0.13857154491934,
0.579164825266405));
#16435=CARTESIAN_POINT('Ctrl Pts',(-0.0957036897026042,0.092147346049863,
0.586236176709736));
#16436=CARTESIAN_POINT('Ctrl Pts',(-0.117475624432153,0.0262528025703711,
0.590660138778806));
#16437=CARTESIAN_POINT('Ctrl Pts',(-0.11766919235599,-9.26074537421669E-5,
0.592436711473616));
#16438=CARTESIAN_POINT('Origin',(0.,0.,-0.0924367114736175));
#16439=CARTESIAN_POINT('',(-0.117794891956694,-0.000106411733115368,0.482563288526384));
#16440=CARTESIAN_POINT('',(-0.117936566864074,5.52347650140707E-5,0.492436711473616));
#16441=CARTESIAN_POINT('',(-0.117775,2.85464118895969E-14,-0.0924367114736175));
#16442=CARTESIAN_POINT('Ctrl Pts',(-0.117794891956694,-0.000106411733115381,
0.482563288526384));
#16443=CARTESIAN_POINT('Ctrl Pts',(-0.117872998614688,-0.00856127641466401,
0.483134981642805));
#16444=CARTESIAN_POINT('Ctrl Pts',(-0.113184542395844,-0.0560672187853419,
0.486353004638329));
#16445=CARTESIAN_POINT('Ctrl Pts',(-0.0487302328423073,-0.130399425645183,
0.492217357512954));
#16446=CARTESIAN_POINT('Ctrl Pts',(0.0831353173341669,-0.111656458896056,
0.50015634715026));
#16447=CARTESIAN_POINT('Ctrl Pts',(0.13889618212661,0.00930034365552528,
0.508095336787567));
#16448=CARTESIAN_POINT('Ctrl Pts',(0.0675071113591811,0.12174331898465,
0.516034326424871));
#16449=CARTESIAN_POINT('Ctrl Pts',(-0.0656800932930844,0.122738629397884,
0.523973316062178));
#16450=CARTESIAN_POINT('Ctrl Pts',(-0.116384786286051,0.04545243224792,
0.529482970096015));
#16451=CARTESIAN_POINT('Ctrl Pts',(-0.117953719733239,0.00325558390455253,
0.53234629425075));
#16452=CARTESIAN_POINT('Ctrl Pts',(-0.117934829819181,5.63106208242166E-5,
0.532563288526383));
#16453=CARTESIAN_POINT('Ctrl Pts',(-0.117936566864074,5.52347650140663E-5,
0.492436711473616));
#16454=CARTESIAN_POINT('Ctrl Pts',(-0.117728017843002,-0.0358510361847084,
0.494872188995279));
#16455=CARTESIAN_POINT('Ctrl Pts',(-0.0810366231971402,-0.111156550628637,
0.499955055891203));
#16456=CARTESIAN_POINT('Ctrl Pts',(0.0471380885036503,-0.131003351527116,
0.507685312161385));
#16457=CARTESIAN_POINT('Ctrl Pts',(0.135643160584381,-0.031381690295376,
0.515627480284167));
#16458=CARTESIAN_POINT('Ctrl Pts',(0.0998851624184703,0.0969888232104648,
0.523569648406945));
#16459=CARTESIAN_POINT('Ctrl Pts',(-0.0273779061153799,0.136507610615132,
0.531511816529727));
#16460=CARTESIAN_POINT('Ctrl Pts',(-0.108290992649607,0.0687756007668377,
0.537800837551949));
#16461=CARTESIAN_POINT('Ctrl Pts',(-0.117713344367368,0.0148299618267192,
0.541442469199912));
#16462=CARTESIAN_POINT('Ctrl Pts',(-0.117629301205424,7.34277634442983E-5,
0.542436711473615));
#16463=CARTESIAN_POINT('Origin',(0.,0.,-0.0924367114736175));
#16464=CARTESIAN_POINT('',(-0.117582256074849,9.06819982020624E-6,0.432563288526383));
#16465=CARTESIAN_POINT('',(-0.11779560903417,-0.000106574656651148,0.442436711473616));
#16466=CARTESIAN_POINT('',(-0.117775,2.85464118895969E-14,-0.0924367114736175));
#16467=CARTESIAN_POINT('Ctrl Pts',(-0.117582256074849,9.06819982019261E-6,
0.432563288526383));
#16468=CARTESIAN_POINT('Ctrl Pts',(-0.117568373935691,-0.020201912089319,
0.43392366903486));
#16469=CARTESIAN_POINT('Ctrl Pts',(-0.10300922874285,-0.0797477867736473,
0.437930379422439));
#16470=CARTESIAN_POINT('Ctrl Pts',(-0.00838939967687663,-0.138954178686792,
0.44458341968912));
#16471=CARTESIAN_POINT('Ctrl Pts',(0.11219917790857,-0.0824013973067221,
0.452522409326426));
#16472=CARTESIAN_POINT('Ctrl Pts',(0.13007709763057,0.0495842159710775,
0.460461398963732));
#16473=CARTESIAN_POINT('Ctrl Pts',(0.0288783492374893,0.136178877755608,
0.468400388601037));
#16474=CARTESIAN_POINT('Ctrl Pts',(-0.0895654556576369,0.100852400902523,
0.475767685121922));
#16475=CARTESIAN_POINT('Ctrl Pts',(-0.117511448025972,0.0305757367622385,
0.480488651763704));
#16476=CARTESIAN_POINT('Ctrl Pts',(-0.117794891956694,-0.000106411733115381,
0.482563288526384));
#16477=CARTESIAN_POINT('Ctrl Pts',(-0.11779560903417,-0.000106574656651151,
0.442436711473616));
#16478=CARTESIAN_POINT('Ctrl Pts',(-0.117873644338608,-0.00854245500997505,
0.443007130042126));
#16479=CARTESIAN_POINT('Ctrl Pts',(-0.113196618671047,-0.056044542179559,
0.446224937984896));
#16480=CARTESIAN_POINT('Ctrl Pts',(-0.0487473834415776,-0.130413074907061,
0.452090135301926));
#16481=CARTESIAN_POINT('Ctrl Pts',(0.0831820848081396,-0.111645054821459,
0.460032303424706));
#16482=CARTESIAN_POINT('Ctrl Pts',(0.138908217753341,0.00940130521287039,
0.467974471547486));
#16483=CARTESIAN_POINT('Ctrl Pts',(0.0673801526530663,0.121835103839429,
0.475916639670265));
#16484=CARTESIAN_POINT('Ctrl Pts',(-0.0658750545035054,0.12265543075329,
0.483858807793047));
#16485=CARTESIAN_POINT('Ctrl Pts',(-0.116424939330292,0.0453161125527027,
0.489365498394162));
#16486=CARTESIAN_POINT('Ctrl Pts',(-0.11795471279604,0.00317945345687678,
0.492224799621019));
#16487=CARTESIAN_POINT('Ctrl Pts',(-0.117936566864074,5.52347650140663E-5,
0.492436711473616));
#16488=CARTESIAN_POINT('Origin',(0.,0.,-0.0924367114736175));
#16489=CARTESIAN_POINT('',(-0.117828183671793,0.000101754196006455,0.382563288526383));
#16490=CARTESIAN_POINT('',(-0.117581664177921,7.09484545444172E-6,0.392436711473616));
#16491=CARTESIAN_POINT('',(-0.117775,2.85464118895969E-14,-0.0924367114736175));
#16492=CARTESIAN_POINT('Ctrl Pts',(-0.117828183671793,0.000101754196006446,
0.382563288526384));
#16493=CARTESIAN_POINT('Ctrl Pts',(-0.117538790254565,-0.0316580736410773,
0.384712356426916));
#16494=CARTESIAN_POINT('Ctrl Pts',(-0.0879068326507716,-0.103002379129266,
0.38950775420655));
#16495=CARTESIAN_POINT('Ctrl Pts',(0.0326876424682324,-0.135315053971568,
0.396949481865287));
#16496=CARTESIAN_POINT('Ctrl Pts',(0.13141703692502,-0.0459152284901983,
0.404888471502591));
#16497=CARTESIAN_POINT('Ctrl Pts',(0.109843140674695,0.0855168418978295,
0.412827461139898));
#16498=CARTESIAN_POINT('Ctrl Pts',(-0.0122846228212416,0.13866410438033,
0.420766450777203));
#16499=CARTESIAN_POINT('Ctrl Pts',(-0.104166535924894,0.0775181589932739,
0.427345059906032));
#16500=CARTESIAN_POINT('Ctrl Pts',(-0.117595378674006,0.0191142356295008,
0.431277339155758));
#16501=CARTESIAN_POINT('Ctrl Pts',(-0.117582256074849,9.06819982019261E-6,
0.432563288526383));
#16502=CARTESIAN_POINT('Ctrl Pts',(-0.117581664177921,7.09484545444172E-6,
0.392436711473616));
#16503=CARTESIAN_POINT('Ctrl Pts',(-0.117570873504463,-0.0200907396801347,
0.393789460463232));
#16504=CARTESIAN_POINT('Ctrl Pts',(-0.10312708440739,-0.079535468422451,
0.397789598827109));
#16505=CARTESIAN_POINT('Ctrl Pts',(-0.00873482453528946,-0.138951719454826,
0.404437126565246));
#16506=CARTESIAN_POINT('Ctrl Pts',(0.112042812448737,-0.0826455423945668,
0.412379294688026));
#16507=CARTESIAN_POINT('Ctrl Pts',(0.130177722634257,0.049372441998279,
0.420321462810806));
#16508=CARTESIAN_POINT('Ctrl Pts',(0.0290564652212241,0.136160197297018,
0.428263630933586));
#16509=CARTESIAN_POINT('Ctrl Pts',(-0.0895090212855029,0.100936776489487,
0.435635380487856));
#16510=CARTESIAN_POINT('Ctrl Pts',(-0.117511471984497,0.0306096014671689,
0.440359740667866));
#16511=CARTESIAN_POINT('Ctrl Pts',(-0.11779560903417,-0.000106574656651151,
0.442436711473616));
#16512=CARTESIAN_POINT('Origin',(0.,0.,-0.0924367114736175));
#16513=CARTESIAN_POINT('',(-0.117911328466355,-7.22474488887591E-5,0.332563288526384));
#16514=CARTESIAN_POINT('',(-0.117821685414254,0.000103165543095151,0.342436711473616));
#16515=CARTESIAN_POINT('',(-0.117775,2.85464118895969E-14,-0.0924367114736175));
#16516=CARTESIAN_POINT('Ctrl Pts',(-0.117911328466355,-7.22474488887752E-5,
0.332563288526384));
#16517=CARTESIAN_POINT('Ctrl Pts',(-0.117942332027964,-0.00437115939612809,
0.332854713939869));
#16518=CARTESIAN_POINT('Ctrl Pts',(-0.115777752883067,-0.0476754067323583,
0.335792469232457));
#16519=CARTESIAN_POINT('Ctrl Pts',(-0.0622106591311991,-0.12453304658572,
0.341376554404146));
#16520=CARTESIAN_POINT('Ctrl Pts',(0.0708961914151981,-0.119801401679107,
0.349315544041452));
#16521=CARTESIAN_POINT('Ctrl Pts',(0.1391024375543,-0.00539978406154301,
0.357254533678757));
#16522=CARTESIAN_POINT('Ctrl Pts',(0.0799699354250877,0.113944965792994,
0.365193523316063));
#16523=CARTESIAN_POINT('Ctrl Pts',(-0.0523695618881846,0.128980908622551,
0.373132512953369));
#16524=CARTESIAN_POINT('Ctrl Pts',(-0.113921748517257,0.0538356345748906,
0.378922434690143));
#16525=CARTESIAN_POINT('Ctrl Pts',(-0.117895144954496,0.00745050051778832,
0.382066026547814));
#16526=CARTESIAN_POINT('Ctrl Pts',(-0.117828183671793,0.000101754196006446,
0.382563288526384));
#16527=CARTESIAN_POINT('Ctrl Pts',(-0.117821685414254,0.000103165543095145,
0.342436711473616));
#16528=CARTESIAN_POINT('Ctrl Pts',(-0.117532262555972,-0.0314544122979593,
0.344571790884339));
#16529=CARTESIAN_POINT('Ctrl Pts',(-0.0882170202347594,-0.102616110661261,
0.349354259669323));
#16530=CARTESIAN_POINT('Ctrl Pts',(0.0320320385160992,-0.135491055083419,
0.356784117828566));
#16531=CARTESIAN_POINT('Ctrl Pts',(0.131227975626944,-0.0465090949381858,
0.364726285951346));
#16532=CARTESIAN_POINT('Ctrl Pts',(0.110205605501345,0.0850799742312894,
0.372668454074126));
#16533=CARTESIAN_POINT('Ctrl Pts',(-0.0117764211155082,0.138727046407055,
0.380610622196906));
#16534=CARTESIAN_POINT('Ctrl Pts',(-0.10403099481448,0.0777947493501838,
0.387200041330069));
#16535=CARTESIAN_POINT('Ctrl Pts',(-0.117591991327853,0.019241607989002,
0.391142071088973));
#16536=CARTESIAN_POINT('Ctrl Pts',(-0.117581664177921,7.09484545444172E-6,
0.392436711473616));
#16537=CARTESIAN_POINT('Origin',(0.,0.,-0.0924367114736175));
#16538=CARTESIAN_POINT('',(-0.117608153246896,-5.64262068778628E-5,0.282563288526383));
#16539=CARTESIAN_POINT('',(-0.117918861549493,-6.80329776671096E-5,0.292436711473615));
#16540=CARTESIAN_POINT('',(-0.117775,2.85464118895969E-14,-0.0924367114736175));
#16541=CARTESIAN_POINT('Ctrl Pts',(-0.117608153246896,-5.64262068778604E-5,
0.282563288526383));
#16542=CARTESIAN_POINT('Ctrl Pts',(-0.117677606263852,-0.0160946837114709,
0.283643401331924));
#16543=CARTESIAN_POINT('Ctrl Pts',(-0.107144424846824,-0.0713401098021974,
0.287369844016567));
#16544=CARTESIAN_POINT('Ctrl Pts',(-0.0229969941138309,-0.137294515779738,
0.293742616580312));
#16545=CARTESIAN_POINT('Ctrl Pts',(0.102883268653204,-0.0937746172089793,
0.301681606217617));
#16546=CARTESIAN_POINT('Ctrl Pts',(0.134580950019115,0.0355895166223291,
0.309620595854923));
#16547=CARTESIAN_POINT('Ctrl Pts',(0.0430789950773988,0.13237388709478,
0.317559585492229));
#16548=CARTESIAN_POINT('Ctrl Pts',(-0.0830523456774332,0.10887452531409,
0.325207149716049));
#16549=CARTESIAN_POINT('Ctrl Pts',(-0.11766079978112,0.0346657214219864,
0.330208384060767));
#16550=CARTESIAN_POINT('Ctrl Pts',(-0.117911328466355,-7.22474488887752E-5,
0.332563288526384));
#16551=CARTESIAN_POINT('Ctrl Pts',(-0.117918861549493,-6.80329776671157E-5,
0.292436711473616));
#16552=CARTESIAN_POINT('Ctrl Pts',(-0.117946256357307,-0.00405052459867665,
0.292706731931186));
#16553=CARTESIAN_POINT('Ctrl Pts',(-0.11595553950755,-0.0470512577090033,
0.295624141763016));
#16554=CARTESIAN_POINT('Ctrl Pts',(-0.0631725212350128,-0.124068972994571,
0.301188940969106));
#16555=CARTESIAN_POINT('Ctrl Pts',(0.0700327441786229,-0.12032993078169,
0.309131109091886));
#16556=CARTESIAN_POINT('Ctrl Pts',(0.139080821187468,-0.00635631000930847,
0.317073277214666));
#16557=CARTESIAN_POINT('Ctrl Pts',(0.0807165776729536,0.11344034374014,
0.325015445337446));
#16558=CARTESIAN_POINT('Ctrl Pts',(-0.0515923433190751,0.129313988454311,
0.332957613460226));
#16559=CARTESIAN_POINT('Ctrl Pts',(-0.113774867115171,0.0543021652640841,
0.338764702172283));
#16560=CARTESIAN_POINT('Ctrl Pts',(-0.117891132111753,0.00767537174388221,
0.341924401510079));
#16561=CARTESIAN_POINT('Ctrl Pts',(-0.117821685414254,0.000103165543095145,
0.342436711473616));
#16562=CARTESIAN_POINT('Origin',(0.,0.,-0.0924367114736175));
#16563=CARTESIAN_POINT('',(-0.117705188630573,0.000102098618198066,0.232563288526383));
#16564=CARTESIAN_POINT('',(-0.1176142238744,-6.23262858038681E-5,0.242436711473616));
#16565=CARTESIAN_POINT('',(-0.117775,2.85464118895969E-14,-0.0924367114736175));
#16566=CARTESIAN_POINT('Ctrl Pts',(-0.117705188630573,0.000102098618198071,
0.232563288526383));
#16567=CARTESIAN_POINT('Ctrl Pts',(-0.117475649963863,-0.0275896003179174,
0.234432088723979));
#16568=CARTESIAN_POINT('Ctrl Pts',(-0.0938913217252411,-0.0948462909608301,
0.238947218800678));
#16569=CARTESIAN_POINT('Ctrl Pts',(0.0182347644767634,-0.138007750384372,
0.246108678756477));
#16570=CARTESIAN_POINT('Ctrl Pts',(0.125841858853055,-0.0595186723796334,
0.254047668393783));
#16571=CARTESIAN_POINT('Ctrl Pts',(0.118249355954961,0.073455671106145,
0.261986658031089));
#16572=CARTESIAN_POINT('Ctrl Pts',(0.00240767183786234,0.139186381940956,
0.269925647668394));
#16573=CARTESIAN_POINT('Ctrl Pts',(-0.0995777503027144,0.0858938305448248,
0.27678452450016));
#16574=CARTESIAN_POINT('Ctrl Pts',(-0.117507442931816,0.0231998416616275,
0.280997071452822));
#16575=CARTESIAN_POINT('Ctrl Pts',(-0.117608153246896,-5.64262068778604E-5,
0.282563288526383));
#16576=CARTESIAN_POINT('Ctrl Pts',(-0.1176142238744,-6.2326285803882E-5,
0.242436711473616));
#16577=CARTESIAN_POINT('Ctrl Pts',(-0.117689148257971,-0.0156863246439697,
0.243489062352292));
#16578=CARTESIAN_POINT('Ctrl Pts',(-0.107519643382358,-0.0705218816827611,
0.247188802605229));
#16579=CARTESIAN_POINT('Ctrl Pts',(-0.024381182195918,-0.137074561658528,
0.253535932232426));
#16580=CARTESIAN_POINT('Ctrl Pts',(0.101985705091022,-0.094777599970642,
0.261478100355206));
#16581=CARTESIAN_POINT('Ctrl Pts',(0.134923209124943,0.0343453801629359,
0.269420268477986));
#16582=CARTESIAN_POINT('Ctrl Pts',(0.0442571924125319,0.132004463632409,
0.277362436600766));
#16583=CARTESIAN_POINT('Ctrl Pts',(-0.0824920331482911,0.109525057495754,
0.285034584265976));
#16584=CARTESIAN_POINT('Ctrl Pts',(-0.117677666622401,0.0349954280503056,
0.290059342556926));
#16585=CARTESIAN_POINT('Ctrl Pts',(-0.117918861549493,-6.80329776671157E-5,
0.292436711473616));
#16586=CARTESIAN_POINT('Origin',(0.,0.,-0.0924367114736175));
#16587=CARTESIAN_POINT('',(-0.117967994073432,-3.0724305424694E-6,0.182563288526383));
#16588=CARTESIAN_POINT('',(-0.117691121003631,9.91971943564221E-5,0.192436711473615));
#16589=CARTESIAN_POINT('',(-0.117775,2.85464118895969E-14,-0.0924367114736175));
#16590=CARTESIAN_POINT('Ctrl Pts',(-0.117967994073432,-3.07243054247449E-6,
0.182563288526383));
#16591=CARTESIAN_POINT('Ctrl Pts',(-0.117968057042159,-0.000167453844217198,
0.182574446236933));
#16592=CARTESIAN_POINT('Ctrl Pts',(-0.117893299674953,-0.0393189363008842,
0.185231933826584));
#16593=CARTESIAN_POINT('Ctrl Pts',(-0.0749972298318695,-0.11727771015962,
0.190535751295337));
#16594=CARTESIAN_POINT('Ctrl Pts',(0.0578663373665801,-0.126610160769685,
0.198474740932643));
#16595=CARTESIAN_POINT('Ctrl Pts',(0.13775723856723,-0.0200396862227523,
0.206413730569949));
#16596=CARTESIAN_POINT('Ctrl Pts',(0.091540828968026,0.104875747581476,
0.214352720207254));
#16597=CARTESIAN_POINT('Ctrl Pts',(-0.0384749358425138,0.133784622116252,
0.22229170984456));
#16598=CARTESIAN_POINT('Ctrl Pts',(-0.110955338697302,0.0622468391270206,
0.22836189928427));
#16599=CARTESIAN_POINT('Ctrl Pts',(-0.11780069007939,0.0116234575531164,
0.231785758844877));
#16600=CARTESIAN_POINT('Ctrl Pts',(-0.117705188630573,0.000102098618198071,
0.232563288526383));
#16601=CARTESIAN_POINT('Ctrl Pts',(-0.117691121003631,9.91971943564221E-5,
0.192436711473615));
#16602=CARTESIAN_POINT('Ctrl Pts',(-0.117474218986382,-0.0270951350261672,
0.194271392773399));
#16603=CARTESIAN_POINT('Ctrl Pts',(-0.0945676524372527,-0.0938598508209937,
0.198753463447442));
#16604=CARTESIAN_POINT('Ctrl Pts',(0.0165156171993534,-0.138242945169174,
0.205882923495746));
#16605=CARTESIAN_POINT('Ctrl Pts',(0.125131592687617,-0.061040658666823,
0.213825091618526));
#16606=CARTESIAN_POINT('Ctrl Pts',(0.119114174013628,0.0720811421096423,
0.221767259741306));
#16607=CARTESIAN_POINT('Ctrl Pts',(0.0039759348809324,0.139169211541763,
0.229709427864086));
#16608=CARTESIAN_POINT('Ctrl Pts',(-0.0990660356104632,0.0867677816679632,
0.236599245108189));
#16609=CARTESIAN_POINT('Ctrl Pts',(-0.117500661679058,0.0236188235484957,
0.240841672978032));
#16610=CARTESIAN_POINT('Ctrl Pts',(-0.1176142238744,-6.2326285803882E-5,
0.242436711473616));
#16611=CARTESIAN_POINT('Origin',(0.,0.,-0.0924367114736175));
#16612=CARTESIAN_POINT('',(-0.117696212882312,-0.000100181105204699,0.132563288526383));
#16613=CARTESIAN_POINT('',(-0.117967699956222,8.3697257429456E-6,0.142436711473616));
#16614=CARTESIAN_POINT('',(-0.117775,2.85464118895969E-14,-0.0924367114736175));
#16615=CARTESIAN_POINT('Ctrl Pts',(-0.117696212882312,-0.000100181105204706,
0.132563288526383));
#16616=CARTESIAN_POINT('Ctrl Pts',(-0.117792074781153,-0.0119544960022407,
0.133363133628988));
#16617=CARTESIAN_POINT('Ctrl Pts',(-0.110696412003459,-0.0629173266909915,
0.136809308610694));
#16618=CARTESIAN_POINT('Ctrl Pts',(-0.0373480950846616,-0.134103559412242,
0.142901813471503));
#16619=CARTESIAN_POINT('Ctrl Pts',(0.0924198687735613,-0.104101940294199,
0.150840803108809));
#16620=CARTESIAN_POINT('Ctrl Pts',(0.137583777756591,0.0211978768359354,
0.158779792746114));
#16621=CARTESIAN_POINT('Ctrl Pts',(0.0567991668878991,0.127092487218924,
0.16671878238342));
#16622=CARTESIAN_POINT('Ctrl Pts',(-0.0757945745091616,0.116657324056303,
0.174646614310176));
#16623=CARTESIAN_POINT('Ctrl Pts',(-0.117953122434976,0.0388197061692436,
0.179928116357831));
#16624=CARTESIAN_POINT('Ctrl Pts',(-0.117967994073432,-3.07243054247449E-6,
0.182563288526383));
#16625=CARTESIAN_POINT('Ctrl Pts',(-0.117967699956222,8.3697257429579E-6,
0.142436711473616));
#16626=CARTESIAN_POINT('Ctrl Pts',(-0.117928252023989,-0.038547130539091,
0.145053723194506));
#16627=CARTESIAN_POINT('Ctrl Pts',(-0.0762804946418446,-0.116178754198862,
0.150318124289656));
#16628=CARTESIAN_POINT('Ctrl Pts',(0.0559861945572589,-0.127473226882309,
0.158229914759066));
#16629=CARTESIAN_POINT('Ctrl Pts',(0.137471621702818,-0.0220324926503626,
0.166172082881846));
#16630=CARTESIAN_POINT('Ctrl Pts',(0.0930189202108026,0.103592267873211,
0.174114251004626));
#16631=CARTESIAN_POINT('Ctrl Pts',(-0.0366486683060043,0.134315868829211,
0.182056419127406));
#16632=CARTESIAN_POINT('Ctrl Pts',(-0.110544190454925,0.0633195416932908,
0.188163905950403));
#16633=CARTESIAN_POINT('Ctrl Pts',(-0.11778720200735,0.0121454601492482,
0.191624003399139));
#16634=CARTESIAN_POINT('Ctrl Pts',(-0.117691121003631,9.91971943564221E-5,
0.192436711473615));
#16635=CARTESIAN_POINT('Origin',(0.,0.,-0.0924367114736175));
#16636=CARTESIAN_POINT('',(-0.117613109409711,6.11591708146705E-5,0.0825632885263832));
#16637=CARTESIAN_POINT('',(-0.117715749944134,-0.000104199409386274,0.0924367114736155));
#16638=CARTESIAN_POINT('',(-0.117775,2.85464118895969E-14,-0.0924367114736175));
#16639=CARTESIAN_POINT('Ctrl Pts',(-0.117613109409711,6.11591708146765E-5,
0.0825632885263832));
#16640=CARTESIAN_POINT('Ctrl Pts',(-0.117502393620717,-0.0235240259785673,
0.0841518210210431));
#16641=CARTESIAN_POINT('Ctrl Pts',(-0.0991849320095013,-0.0865581493706475,
0.088386683394805));
#16642=CARTESIAN_POINT('Ctrl Pts',(0.00357853460314598,-0.139161043603659,
0.0952678756476685));
#16643=CARTESIAN_POINT('Ctrl Pts',(0.118863112008681,-0.0724583686054966,
0.103206865284975));
#16644=CARTESIAN_POINT('Ctrl Pts',(0.125336705278751,0.0605752693714656,
0.11114585492228));
#16645=CARTESIAN_POINT('Ctrl Pts',(0.0170731091066207,0.138156245709763,
0.119084844559586));
#16646=CARTESIAN_POINT('Ctrl Pts',(-0.094337657277608,0.0941904991302726,
0.126223989094287));
#16647=CARTESIAN_POINT('Ctrl Pts',(-0.11747491061231,0.0272661325996615,
0.130716803749886));
#16648=CARTESIAN_POINT('Ctrl Pts',(-0.117696212882312,-0.000100181105204706,
0.132563288526383));
#16649=CARTESIAN_POINT('Ctrl Pts',(-0.117715749944134,-0.000104199409386274,
0.0924367114736155));
#16650=CARTESIAN_POINT('Ctrl Pts',(-0.117810584636384,-0.011244028442556,
0.0931886642413524));
#16651=CARTESIAN_POINT('Ctrl Pts',(-0.111246641208053,-0.0614941526881817,
0.0965880063833492));
#16652=CARTESIAN_POINT('Ctrl Pts',(-0.0397151780004399,-0.133441281507892,
0.102634737899606));
#16653=CARTESIAN_POINT('Ctrl Pts',(0.0906220264938673,-0.105695447092796,
0.110576906022386));
#16654=CARTESIAN_POINT('Ctrl Pts',(0.137940159127448,0.0188783162799928,
0.118519074145166));
#16655=CARTESIAN_POINT('Ctrl Pts',(0.0588909273047484,0.126157580947307,
0.126461242267946));
#16656=CARTESIAN_POINT('Ctrl Pts',(-0.074108440039672,0.117863552156501,
0.134403410390726));
#16657=CARTESIAN_POINT('Ctrl Pts',(-0.117763087033452,0.0399060678969832,
0.139728566792616));
#16658=CARTESIAN_POINT('Ctrl Pts',(-0.117968157858494,0.000455912857932787,
0.142406333820246));
#16659=CARTESIAN_POINT('Ctrl Pts',(-0.117967699956222,8.3697257429579E-6,
0.142436711473616));
#16660=CARTESIAN_POINT('Origin',(0.,0.,-0.0924367114736175));
#16661=CARTESIAN_POINT('',(-0.117917485785546,7.60014832213593E-5,0.0325632885263832));
#16662=CARTESIAN_POINT('',(-0.117600989619072,5.04992496179954E-5,0.0424367114736154));
#16663=CARTESIAN_POINT('',(-0.117775,2.85464118895969E-14,-0.0924367114736175));
#16664=CARTESIAN_POINT('Ctrl Pts',(-0.117917485785546,7.60014832213644E-5,
0.0325632885263832));
#16665=CARTESIAN_POINT('Ctrl Pts',(-0.117676727567847,-0.0349830640657269,
0.0349405084130983));
#16666=CARTESIAN_POINT('Ctrl Pts',(-0.0825043195215805,-0.109517225708346,
0.0399640581789154));
#16667=CARTESIAN_POINT('Ctrl Pts',(0.0441923146003338,-0.131999388615902,
0.0476339378238343));
#16668=CARTESIAN_POINT('Ctrl Pts',(0.134874939024977,-0.034459980695041,
0.0555729274611401));
#16669=CARTESIAN_POINT('Ctrl Pts',(0.102091080224759,0.094638871230671,
0.0635119170984456));
#16670=CARTESIAN_POINT('Ctrl Pts',(-0.0241513666277066,0.137095110112719,
0.0714509067357516));
#16671=CARTESIAN_POINT('Ctrl Pts',(-0.107448046275642,0.0706698818446754,
0.0778013638783972));
#16672=CARTESIAN_POINT('Ctrl Pts',(-0.117686834607281,0.0157664388843013,
0.0815054911419412));
#16673=CARTESIAN_POINT('Ctrl Pts',(-0.117613109409711,6.11591708146765E-5,
0.0825632885263832));
#16674=CARTESIAN_POINT('Ctrl Pts',(-0.117600989619072,5.04992496179954E-5,
0.0424367114736154));
#16675=CARTESIAN_POINT('Ctrl Pts',(-0.117514779739531,-0.0227353060542692,
0.043970994662459));
#16676=CARTESIAN_POINT('Ctrl Pts',(-0.100129952091853,-0.0849605109884783,
0.0481526672255625));
#16677=CARTESIAN_POINT('Ctrl Pts',(0.000787973702835166,-0.139222729671589,
0.054981729162926));
#16678=CARTESIAN_POINT('Ctrl Pts',(0.117431922513572,-0.0747907597173192,
0.0629238972857061));
#16679=CARTESIAN_POINT('Ctrl Pts',(0.126496838785129,0.0581591461343325,
0.070866065408486));
#16680=CARTESIAN_POINT('Ctrl Pts',(0.0196773008918215,0.137828289815661,
0.0788082335312661));
#16681=CARTESIAN_POINT('Ctrl Pts',(-0.0933482651079043,0.0956446566614129,
0.085998448886309));
#16682=CARTESIAN_POINT('Ctrl Pts',(-0.11747670148927,0.0279758085988667,
0.0905412748670923));
#16683=CARTESIAN_POINT('Ctrl Pts',(-0.117715749944134,-0.000104199409386274,
0.0924367114736155));
#16684=CARTESIAN_POINT('Origin',(0.,0.,1.55));
#16685=CARTESIAN_POINT('',(-0.143211704627722,-5.70397197726547E-6,1.50700023576178));
#16686=CARTESIAN_POINT('Ctrl Pts',(-0.0334019664626774,0.112939183906323,
1.532225));
#16687=CARTESIAN_POINT('Ctrl Pts',(-0.0250606930336426,0.115799676338094,
1.53184761307169));
#16688=CARTESIAN_POINT('Ctrl Pts',(-0.0164287086124659,0.117635554524944,
1.53147359869818));
#16689=CARTESIAN_POINT('Ctrl Pts',(-0.00767226928320402,0.118510614220874,
1.53110056493424));
#16690=CARTESIAN_POINT('Ctrl Pts',(-0.0042150196872779,0.118856108509867,
1.53095328237096));
#16691=CARTESIAN_POINT('Ctrl Pts',(-0.000736351480830917,0.119051293525916,
1.53080607672538));
#16692=CARTESIAN_POINT('Ctrl Pts',(0.00274830211697625,0.119097943881266,
1.53065904037218));
#16693=CARTESIAN_POINT('Ctrl Pts',(0.00972321854123044,0.119191319684798,
1.53036473098213));
#16694=CARTESIAN_POINT('Ctrl Pts',(0.0166907125456733,0.118690968429664,
1.53007241075126));
#16695=CARTESIAN_POINT('Ctrl Pts',(0.0235721318645625,0.11762150546261,
1.52978094357425));
#16696=CARTESIAN_POINT('Ctrl Pts',(0.0273478463565568,0.117034709826966,
1.52962102062912));
#16697=CARTESIAN_POINT('Ctrl Pts',(0.0310977188904398,0.116276259986281,
1.52946135449799));
#16698=CARTESIAN_POINT('Ctrl Pts',(0.0348087249896146,0.115347945392283,
1.52930175751644));
#16699=CARTESIAN_POINT('Ctrl Pts',(0.0378768737129624,0.114580442682688,
1.52916980751093));
#16700=CARTESIAN_POINT('Ctrl Pts',(0.0409182562642153,0.113696477767379,
1.52903790896105));
#16701=CARTESIAN_POINT('Ctrl Pts',(0.0439120268522727,0.112701821307647,
1.52890655030309));
#16702=CARTESIAN_POINT('Ctrl Pts',(0.0504861734289241,0.110517613410832,
1.52861809430882));
#16703=CARTESIAN_POINT('Ctrl Pts',(0.0568477403450367,0.107796947733889,
1.528331525126));
#16704=CARTESIAN_POINT('Ctrl Pts',(0.0629211062797432,0.10455513280498,
1.52804576869741));
#16705=CARTESIAN_POINT('Ctrl Pts',(0.0667529140263229,0.102509807084265,
1.52786547926507));
#16706=CARTESIAN_POINT('Ctrl Pts',(0.0704699809867569,0.100256700264741,
1.52768551335768));
#16707=CARTESIAN_POINT('Ctrl Pts',(0.0740519796445933,0.0977963961590643,
1.52750560123222));
#16708=CARTESIAN_POINT('Ctrl Pts',(0.0761474027326905,0.0963571499395001,
1.52740035495562));
#16709=CARTESIAN_POINT('Ctrl Pts',(0.0781972522873126,0.0948464165467323,
1.52729509152825));
#16710=CARTESIAN_POINT('Ctrl Pts',(0.0801950758490376,0.0932655888959708,
1.52718986717129));
#16711=CARTESIAN_POINT('Ctrl Pts',(0.0872135629190184,0.0877120362002772,
1.52682020700562));
#16712=CARTESIAN_POINT('Ctrl Pts',(0.0935342345834078,0.0813437113039547,
1.52645409167081));
#16713=CARTESIAN_POINT('Ctrl Pts',(0.0991216768718319,0.0743433873765979,
1.52608928877518));
#16714=CARTESIAN_POINT('Ctrl Pts',(0.101857856375295,0.0709153174549959,
1.52591064420861));
#16715=CARTESIAN_POINT('Ctrl Pts',(0.104417791592617,0.0673349702414553,
1.52573231437502));
#16716=CARTESIAN_POINT('Ctrl Pts',(0.106794530290299,0.0636205708890664,
1.52555403711528));
#16717=CARTESIAN_POINT('Ctrl Pts',(0.108394385735532,0.0611202951812291,
1.52543403324399));
#16718=CARTESIAN_POINT('Ctrl Pts',(0.109912312880749,0.0585571637778213,
1.52531395827658));
#16719=CARTESIAN_POINT('Ctrl Pts',(0.111341951189028,0.0559432008961949,
1.5251940432238));
#16720=CARTESIAN_POINT('Ctrl Pts',(0.115894033640165,0.0476201345006791,
1.52481222412716));
#16721=CARTESIAN_POINT('Ctrl Pts',(0.119530893641226,0.0388304356906876,
1.52443409356659));
#16722=CARTESIAN_POINT('Ctrl Pts',(0.122195159250079,0.0297595052710396,
1.52405718851832));
#16723=CARTESIAN_POINT('Ctrl Pts',(0.123464283518865,0.0254385629829291,
1.52387764960816));
#16724=CARTESIAN_POINT('Ctrl Pts',(0.124512110981915,0.0210533134598664,
1.52369838877875));
#16725=CARTESIAN_POINT('Ctrl Pts',(0.12532867129748,0.0166220814218575,
1.52351913980531));
#16726=CARTESIAN_POINT('Ctrl Pts',(0.126067828800149,0.012610891624201,
1.52335688207487));
#16727=CARTESIAN_POINT('Ctrl Pts',(0.12661735951473,0.00855739899605222,
1.52319445303817));
#16728=CARTESIAN_POINT('Ctrl Pts',(0.126966826155483,0.00450415768051923,
1.52303280899981));
#16729=CARTESIAN_POINT('Ctrl Pts',(0.127602972227412,-0.00287409603749457,
1.52273856283131));
#16730=CARTESIAN_POINT('Ctrl Pts',(0.12758177643555,-0.010267620141741,
1.52244625042084));
#16731=CARTESIAN_POINT('Ctrl Pts',(0.126865581413421,-0.0175939782534482,
1.52215473434257));
#16732=CARTESIAN_POINT('Ctrl Pts',(0.126426462283551,-0.0220859726121444,
1.52197599770985));
#16733=CARTESIAN_POINT('Ctrl Pts',(0.12572570473317,-0.0265528301690258,
1.52179756043894));
#16734=CARTESIAN_POINT('Ctrl Pts',(0.124776542651163,-0.0309793260681717,
1.52161916036391));
#16735=CARTESIAN_POINT('Ctrl Pts',(0.124151644840291,-0.0338935887106027,
1.52150170748789));
#16736=CARTESIAN_POINT('Ctrl Pts',(0.123418330834614,-0.0367926408403149,
1.52138417707714));
#16737=CARTESIAN_POINT('Ctrl Pts',(0.122581975874549,-0.0396644408336013,
1.52126680258073));
#16738=CARTESIAN_POINT('Ctrl Pts',(0.120074191833131,-0.0482754427851461,
1.52091485884509));
#16739=CARTESIAN_POINT('Ctrl Pts',(0.116656903439717,-0.0566007293654626,
1.52056600333313));
#16740=CARTESIAN_POINT('Ctrl Pts',(0.112443760417108,-0.0645262187619275,
1.52021830866717));
#16741=CARTESIAN_POINT('Ctrl Pts',(0.109356904590302,-0.0703330102694749,
1.51996356219884));
#16742=CARTESIAN_POINT('Ctrl Pts',(0.105841781173658,-0.0759253337267248,
1.51970943888381));
#16743=CARTESIAN_POINT('Ctrl Pts',(0.101930367117466,-0.0812537151913617,
1.51945518067311));
#16744=CARTESIAN_POINT('Ctrl Pts',(0.100130771446666,-0.0837052409256295,
1.51933819945644));
#16745=CARTESIAN_POINT('Ctrl Pts',(0.0982476276828181,-0.0860996963839449,
1.51922123442864));
#16746=CARTESIAN_POINT('Ctrl Pts',(0.0962924325256194,-0.0884227179472683,
1.51910469697823));
#16747=CARTESIAN_POINT('Ctrl Pts',(0.0906946176521128,-0.0950736369671782,
1.51877104482549));
#16748=CARTESIAN_POINT('Ctrl Pts',(0.0844921899154374,-0.101162815315101,
1.51843983772287));
#16749=CARTESIAN_POINT('Ctrl Pts',(0.0777644521522082,-0.106582693579069,
1.51810941878));
#16750=CARTESIAN_POINT('Ctrl Pts',(0.0731067700043679,-0.110334931124879,
1.5178806663426));
#16751=CARTESIAN_POINT('Ctrl Pts',(0.0681966627772886,-0.113766151308436,
1.51765229166508));
#16752=CARTESIAN_POINT('Ctrl Pts',(0.0630541948599911,-0.116833686038022,
1.5174237449583));
#16753=CARTESIAN_POINT('Ctrl Pts',(0.0607686815400033,-0.118197018118406,
1.51732216988754));
#16754=CARTESIAN_POINT('Ctrl Pts',(0.0584414404741937,-0.119485783651375,
1.51722075040181));
#16755=CARTESIAN_POINT('Ctrl Pts',(0.0560784264268894,-0.12069488199044,
1.51711960151386));
#16756=CARTESIAN_POINT('Ctrl Pts',(0.0475595529450054,-0.125053787850271,
1.51675495087613));
#16757=CARTESIAN_POINT('Ctrl Pts',(0.038563113830939,-0.128389854466075,
1.51639315730301));
#16758=CARTESIAN_POINT('Ctrl Pts',(0.0292711048986314,-0.130741856378471,
1.51603205677802));
#16759=CARTESIAN_POINT('Ctrl Pts',(0.0254547302664753,-0.13170786066222,
1.51588374709674));
#16760=CARTESIAN_POINT('Ctrl Pts',(0.0215881861914954,-0.132507324978224,
1.51573555432397));
#16761=CARTESIAN_POINT('Ctrl Pts',(0.0176832233642019,-0.13314066674995,
1.51558732853105));
#16762=CARTESIAN_POINT('Ctrl Pts',(0.0144414794405867,-0.133666441752394,
1.51546427740745));
#16763=CARTESIAN_POINT('Ctrl Pts',(0.0111713231872828,-0.134077605234841,
1.5153411329761));
#16764=CARTESIAN_POINT('Ctrl Pts',(0.00789687394913892,-0.134372952697723,
1.51521845803943));
#16765=CARTESIAN_POINT('Ctrl Pts',(-0.00208492598009478,-0.135273287095873,
1.51484449692866));
#16766=CARTESIAN_POINT('Ctrl Pts',(-0.0121386692885745,-0.135107999768821,
1.51447364169918));
#16767=CARTESIAN_POINT('Ctrl Pts',(-0.0220717676774029,-0.133899092645375,
1.51410356562093));
#16768=CARTESIAN_POINT('Ctrl Pts',(-0.0271373055616968,-0.133282591671289,
1.51391483957382));
#16769=CARTESIAN_POINT('Ctrl Pts',(-0.0321716696217597,-0.132393849601707,
1.51372631615657));
#16770=CARTESIAN_POINT('Ctrl Pts',(-0.0371491047637803,-0.131230566976147,
1.51353768678866));
#16771=CARTESIAN_POINT('Ctrl Pts',(-0.0401763453142056,-0.130523066780721,
1.51342296375255));
#16772=CARTESIAN_POINT('Ctrl Pts',(-0.0431793745847511,-0.129714439573166,
1.51330831773957));
#16773=CARTESIAN_POINT('Ctrl Pts',(-0.0461427198170546,-0.128807808452418,
1.51319405707679));
#16774=CARTESIAN_POINT('Ctrl Pts',(-0.0557912886485991,-0.125855842991896,
1.51282202756853));
#16775=CARTESIAN_POINT('Ctrl Pts',(-0.0650506639775802,-0.121862017750276,
1.51245293010828));
#16776=CARTESIAN_POINT('Ctrl Pts',(-0.0737251756215706,-0.116823260910032,
1.51208446868514));
#16777=CARTESIAN_POINT('Ctrl Pts',(-0.0774533877539874,-0.114657657224767,
1.51192610791459));
#16778=CARTESIAN_POINT('Ctrl Pts',(-0.0810733781510443,-0.112298364258586,
1.51176786463208));
#16779=CARTESIAN_POINT('Ctrl Pts',(-0.0845783705992567,-0.109758519633299,
1.51160955655689));
#16780=CARTESIAN_POINT('Ctrl Pts',(-0.0871260289206952,-0.107912394030924,
1.51149448786814));
#16781=CARTESIAN_POINT('Ctrl Pts',(-0.0896122610481647,-0.105970921032248,
1.51137940572563));
#16782=CARTESIAN_POINT('Ctrl Pts',(-0.0920243025666997,-0.10394826075131,
1.51126473391974));
#16783=CARTESIAN_POINT('Ctrl Pts',(-0.0995315444015674,-0.0976529296958118,
1.51090782920982));
#16784=CARTESIAN_POINT('Ctrl Pts',(-0.106349817996106,-0.090554906599088,
1.51055366538392));
#16785=CARTESIAN_POINT('Ctrl Pts',(-0.112409916721278,-0.0828189535999138,
1.51020021897155));
#16786=CARTESIAN_POINT('Ctrl Pts',(-0.11567060314877,-0.0786565598680515,
1.51001004419521));
#16787=CARTESIAN_POINT('Ctrl Pts',(-0.118711357121208,-0.0743087544864998,
1.50982007711492));
#16788=CARTESIAN_POINT('Ctrl Pts',(-0.121517490738653,-0.0697974244982526,
1.50963000253165));
#16789=CARTESIAN_POINT('Ctrl Pts',(-0.123184827969132,-0.0671169005197731,
1.50951706477726));
#16790=CARTESIAN_POINT('Ctrl Pts',(-0.124768226583796,-0.064379797453554,
1.50940414472167));
#16791=CARTESIAN_POINT('Ctrl Pts',(-0.12625918933752,-0.0616017405091787,
1.50929161182319));
#16792=CARTESIAN_POINT('Ctrl Pts',(-0.131254477666307,-0.0522942005345653,
1.50891458411209));
#16793=CARTESIAN_POINT('Ctrl Pts',(-0.135235816373665,-0.0424980109473837,
1.50854057440173));
#16794=CARTESIAN_POINT('Ctrl Pts',(-0.138100316247284,-0.0323932585971084,
1.50816719719795));
#16795=CARTESIAN_POINT('Ctrl Pts',(-0.139428601593765,-0.027707625827389,
1.5079940600046));
#16796=CARTESIAN_POINT('Ctrl Pts',(-0.140516076092011,-0.0229552175461711,
1.50782105881478));
#16797=CARTESIAN_POINT('Ctrl Pts',(-0.14134846970832,-0.01815262603916,
1.50764795577689));
#16798=CARTESIAN_POINT('Ctrl Pts',(-0.141840021659925,-0.0153165600461233,
1.5075457335416));
#16799=CARTESIAN_POINT('Ctrl Pts',(-0.142241997144177,-0.0124651428186592,
1.50744355431084));
#16800=CARTESIAN_POINT('Ctrl Pts',(-0.142550993842162,-0.00961078035088443,
1.50734168592779));
#16801=CARTESIAN_POINT('Ctrl Pts',(-0.142847161918882,-0.00687492249914849,
1.50724404681617));
#16802=CARTESIAN_POINT('Ctrl Pts',(-0.143058332724879,-0.00413406598225375,
1.5071466105924));
#16803=CARTESIAN_POINT('Ctrl Pts',(-0.143182669649515,-0.00139134585336764,
1.50704933585643));
#16804=CARTESIAN_POINT('Ctrl Pts',(-0.143203595382121,-0.00092974984559876,
1.50703296465278));
#16805=CARTESIAN_POINT('Ctrl Pts',(-0.143222061023464,-0.000468100854706259,
1.50701659802318));
#16806=CARTESIAN_POINT('Ctrl Pts',(-0.143238079070951,-6.41379011939899E-6,
1.50700023577028));
#16807=CARTESIAN_POINT('',(-0.00156744678985144,0.146109855568756,1.50365));
#16808=CARTESIAN_POINT('Ctrl Pts',(-0.00156962371672063,0.146072546381438,
1.50365));
#16809=CARTESIAN_POINT('Ctrl Pts',(-0.011711474284147,0.144648739717271,
1.50495065132295));
#16810=CARTESIAN_POINT('Ctrl Pts',(-0.0216501921041044,0.142222471223284,
1.50626105010813));
#16811=CARTESIAN_POINT('Ctrl Pts',(-0.0312062965385204,0.138804788898175,
1.50759029209282));
#16812=CARTESIAN_POINT('Ctrl Pts',(-0.0379863325344082,0.136379950477271,
1.50853338648503));
#16813=CARTESIAN_POINT('Ctrl Pts',(-0.0445735484268955,0.133455002060128,
1.5094859663039));
#16814=CARTESIAN_POINT('Ctrl Pts',(-0.0508923708069948,0.130021662144985,
1.51045128011208));
#16815=CARTESIAN_POINT('Ctrl Pts',(-0.053607485163773,0.128546401418451,
1.51086606268101));
#16816=CARTESIAN_POINT('Ctrl Pts',(-0.0562647183424556,0.126981576978965,
1.51128195276517));
#16817=CARTESIAN_POINT('Ctrl Pts',(-0.0588579379029418,0.125328026221608,
1.51169910067666));
#16818=CARTESIAN_POINT('Ctrl Pts',(-0.0624505046767585,0.123037247762191,
1.51227700458785));
#16819=CARTESIAN_POINT('Ctrl Pts',(-0.0659209207101175,0.120575889029892,
1.51285741907924));
#16820=CARTESIAN_POINT('Ctrl Pts',(-0.0692542752175272,0.117943487410649,
1.51344114883776));
#16821=CARTESIAN_POINT('Ctrl Pts',(-0.0735613784355843,0.114542101371374,
1.51419539934302));
#16822=CARTESIAN_POINT('Ctrl Pts',(-0.0776398170223455,0.110855132244726,
1.51495518495604));
#16823=CARTESIAN_POINT('Ctrl Pts',(-0.0814741368103916,0.106911749311875,
1.51572224163114));
#16824=CARTESIAN_POINT('Ctrl Pts',(-0.0845038784997064,0.103795829845314,
1.51632834224744));
#16825=CARTESIAN_POINT('Ctrl Pts',(-0.087381117690253,0.10051973853988,
1.51693898261853));
#16826=CARTESIAN_POINT('Ctrl Pts',(-0.0900959757046659,0.0970973798321736,
1.51755501917095));
#16827=CARTESIAN_POINT('Ctrl Pts',(-0.0920052356275281,0.0946905606587243,
1.51798825505079));
#16828=CARTESIAN_POINT('Ctrl Pts',(-0.093830595110286,0.092215607777745,
1.51842338946406));
#16829=CARTESIAN_POINT('Ctrl Pts',(-0.0955653742165971,0.0896840982544811,
1.51885969689116));
#16830=CARTESIAN_POINT('Ctrl Pts',(-0.0997851775729162,0.0835262696618028,
1.51992100293214));
#16831=CARTESIAN_POINT('Ctrl Pts',(-0.103479134251024,0.0770231540939269,
1.52099120961793));
#16832=CARTESIAN_POINT('Ctrl Pts',(-0.106606394578922,0.0702509006766953,
1.52207541818308));
#16833=CARTESIAN_POINT('Ctrl Pts',(-0.108879606303698,0.0653281362576702,
1.52286353153598));
#16834=CARTESIAN_POINT('Ctrl Pts',(-0.110852991156964,0.0602629640702717,
1.52365904329275));
#16835=CARTESIAN_POINT('Ctrl Pts',(-0.112503888351057,0.0550849881514033,
1.524463912762));
#16836=CARTESIAN_POINT('Ctrl Pts',(-0.113450017754745,0.0521174894567802,
1.52492518356294));
#16837=CARTESIAN_POINT('Ctrl Pts',(-0.114289979676541,0.0491121240008169,
1.52538965304266));
#16838=CARTESIAN_POINT('Ctrl Pts',(-0.115015874151616,0.0460903162170444,
1.52585530945224));
#16839=CARTESIAN_POINT('Ctrl Pts',(-0.117053612444637,0.0376074669234184,
1.52716250482259));
#16840=CARTESIAN_POINT('Ctrl Pts',(-0.118206139871793,0.0289652499882669,
1.52848357355921));
#16841=CARTESIAN_POINT('Ctrl Pts',(-0.11838625730212,0.0202925750432425,
1.52982832573377));
#16842=CARTESIAN_POINT('Ctrl Pts',(-0.118492077855379,0.015197303257165,
1.53061837930521));
#16843=CARTESIAN_POINT('Ctrl Pts',(-0.118261361656021,0.0100916471271278,
1.53141660760476));
#16844=CARTESIAN_POINT('Ctrl Pts',(-0.11766859746431,0.00500517689818842,
1.532225));
#16845=CARTESIAN_POINT('',(-0.115079981391543,0.0902137050004572,1.50365));
#16846=CARTESIAN_POINT('Origin',(0.,0.,1.50365));
#16847=CARTESIAN_POINT('Ctrl Pts',(-0.143238079070951,-6.41379011939899E-6,
1.50700023577028));
#16848=CARTESIAN_POINT('Ctrl Pts',(-0.143514357617001,0.00795674345750163,
1.50671802038504));
#16849=CARTESIAN_POINT('Ctrl Pts',(-0.14306421847979,0.0159310909218757,
1.50643710681857));
#16850=CARTESIAN_POINT('Ctrl Pts',(-0.141940608246003,0.023841490005315,
1.50615648267927));
#16851=CARTESIAN_POINT('Ctrl Pts',(-0.141317731836386,0.0282266413964,1.50600091791928));
#16852=CARTESIAN_POINT('Ctrl Pts',(-0.14048752132733,0.0325921818867556,
1.50584544210227));
#16853=CARTESIAN_POINT('Ctrl Pts',(-0.139456452513291,0.0369250818702156,
1.5056898827608));
#16854=CARTESIAN_POINT('Ctrl Pts',(-0.138790989895207,0.0397215809279161,
1.50558948313156));
#16855=CARTESIAN_POINT('Ctrl Pts',(-0.138042009924554,0.0425029011667524,
1.50548910366784));
#16856=CARTESIAN_POINT('Ctrl Pts',(-0.137214434473447,0.0452564915355094,
1.50538902890071));
#16857=CARTESIAN_POINT('Ctrl Pts',(-0.134176751889031,0.0553637675507716,
1.50502169637912));
#16858=CARTESIAN_POINT('Ctrl Pts',(-0.130076454936343,0.0651325632434767,
1.50465723703036));
#16859=CARTESIAN_POINT('Ctrl Pts',(-0.125018127980614,0.0743940890034878,
1.50429344851366));
#16860=CARTESIAN_POINT('Ctrl Pts',(-0.122034683484208,0.0798566160996726,
1.50407888293545));
#16861=CARTESIAN_POINT('Ctrl Pts',(-0.118716925567465,0.0851425936725427,
1.50386455072235));
#16862=CARTESIAN_POINT('Ctrl Pts',(-0.115078604842436,0.0902138214954005,
1.50365));
#16863=CARTESIAN_POINT('',(-0.05,-6.12323399573677E-18,1.6));
#16864=CARTESIAN_POINT('',(-0.1,-1.22464679914735E-17,1.55));
#16865=CARTESIAN_POINT('Origin',(0.,0.,1.6));
#16866=CARTESIAN_POINT('Ctrl Pts',(0.0850780204044575,-0.11908002747757,
-0.0164977839420936));
#16867=CARTESIAN_POINT('Ctrl Pts',(0.124677800165771,-0.0907875342533835,
-0.0138514540629917));
#16868=CARTESIAN_POINT('Ctrl Pts',(0.172751483861701,0.00791416360185712,
-0.00855879430478784));
#16869=CARTESIAN_POINT('Ctrl Pts',(0.0868617128612901,0.149726167188418,
-0.000619804667482127));
#16870=CARTESIAN_POINT('Ctrl Pts',(-0.078614020905812,0.154028602276276,
0.00731918496982359));
#16871=CARTESIAN_POINT('Ctrl Pts',(-0.172087192378165,0.0175525219725009,
0.0152581746071293));
#16872=CARTESIAN_POINT('Ctrl Pts',(-0.108045720411827,-0.135108484733225,
0.0231971642444351));
#16873=CARTESIAN_POINT('Ctrl Pts',(0.0549144151285058,-0.164025561655164,
0.0311361538817407));
#16874=CARTESIAN_POINT('Ctrl Pts',(0.167598788591005,-0.0428207868793744,
0.0390751435190465));
#16875=CARTESIAN_POINT('Ctrl Pts',(0.126860790413016,0.117600499296196,
0.0470141331563521));
#16876=CARTESIAN_POINT('Ctrl Pts',(-0.0300110592737492,0.170357625684536,
0.054953122793658));
#16877=CARTESIAN_POINT('Ctrl Pts',(-0.159409054995301,0.0671687418111174,
0.0628921124309635));
#16878=CARTESIAN_POINT('Ctrl Pts',(-0.142879399887002,-0.0975110083167992,
0.0708311020682695));
#16879=CARTESIAN_POINT('Ctrl Pts',(0.00444677171871267,-0.172924803493063,
0.078770091705575));
#16880=CARTESIAN_POINT('Ctrl Pts',(0.147702113712341,-0.0900384822365835,
0.0867090813428809));
#16881=CARTESIAN_POINT('Ctrl Pts',(0.155746353789385,0.0752722621313087,
0.0946480709801864));
#16882=CARTESIAN_POINT('Ctrl Pts',(0.021215449100004,0.17167621786987,0.102587060617492));
#16883=CARTESIAN_POINT('Ctrl Pts',(-0.132736728465598,0.110922462699857,
0.110526050254798));
#16884=CARTESIAN_POINT('Ctrl Pts',(-0.165177537004225,-0.0513732581591355,
0.118465039892104));
#16885=CARTESIAN_POINT('Ctrl Pts',(-0.0464096261145344,-0.166640254043574,
0.126404029529409));
#16886=CARTESIAN_POINT('Ctrl Pts',(0.114843114370719,-0.129359532685675,
0.134343019166715));
#16887=CARTESIAN_POINT('Ctrl Pts',(0.170964855654229,0.0263409830179588,
0.142282008804021));
#16888=CARTESIAN_POINT('Ctrl Pts',(0.0705799878925336,0.157928129946847,
0.150220998441327));
#16889=CARTESIAN_POINT('Ctrl Pts',(-0.0944160212638482,0.144942899583874,
0.158159988078632));
#16890=CARTESIAN_POINT('Ctrl Pts',(-0.172980633894512,-0.000727622896455919,
0.166098977715938));
#16891=CARTESIAN_POINT('Ctrl Pts',(-0.0931933312323777,-0.145732055885043,
0.174037967353244));
#16892=CARTESIAN_POINT('Ctrl Pts',(0.0719060791645076,-0.157328779695546,
0.181976956990549));
#16893=CARTESIAN_POINT('Ctrl Pts',(0.171180402159323,-0.0249017879745179,
0.189915946627855));
#16894=CARTESIAN_POINT('Ctrl Pts',(0.113750798721884,0.13032108391891,0.197854936265161));
#16895=CARTESIAN_POINT('Ctrl Pts',(-0.0478098650864174,0.16624393501773,
0.205793925902467));
#16896=CARTESIAN_POINT('Ctrl Pts',(-0.16560387403618,0.0499818570245514,
0.213732915539772));
#16897=CARTESIAN_POINT('Ctrl Pts',(-0.131798885878402,-0.112035185581475,
0.221671905177078));
#16898=CARTESIAN_POINT('Ctrl Pts',(0.0226589495323734,-0.171491694067101,
0.229610894814384));
#16899=CARTESIAN_POINT('Ctrl Pts',(0.156374069566079,-0.073959309724122,
0.237549884451689));
#16900=CARTESIAN_POINT('Ctrl Pts',(0.146939445926624,0.0912777539068999,
0.245488874088995));
#16901=CARTESIAN_POINT('Ctrl Pts',(0.00299182995941577,0.172956289510158,
0.253427863726301));
#16902=CARTESIAN_POINT('Ctrl Pts',(-0.143694601292225,0.0963051955349955,
0.261366853363607));
#16903=CARTESIAN_POINT('Ctrl Pts',(-0.15883847309497,-0.0685067047260848,
0.269305843000912));
#16904=CARTESIAN_POINT('Ctrl Pts',(-0.0285766086907934,-0.170605411881679,
0.277244832638218));
#16905=CARTESIAN_POINT('Ctrl Pts',(0.12784518248692,-0.116526556812001,
0.285183822275524));
#16906=CARTESIAN_POINT('Ctrl Pts',(0.167233470900423,0.0442243749325307,
0.293122811912829));
#16907=CARTESIAN_POINT('Ctrl Pts',(0.0535309779628647,0.164490922320707,
0.301061801550136));
#16908=CARTESIAN_POINT('Ctrl Pts',(-0.109175456582181,0.134177303623408,
0.309000791187441));
#16909=CARTESIAN_POINT('Ctrl Pts',(-0.171939242908932,-0.0189664407699395,
0.316939780824747));
#16910=CARTESIAN_POINT('Ctrl Pts',(-0.0773044361184472,-0.154747708493488,
0.324878770462053));
#16911=CARTESIAN_POINT('Ctrl Pts',(0.0880972839194656,-0.148868054644337,
0.332817760099358));
#16912=CARTESIAN_POINT('Ctrl Pts',(0.172851978230285,-0.00670989936239309,
0.340756749736664));
#16913=CARTESIAN_POINT('Ctrl Pts',(0.0993725327910066,0.141590708926387,
0.34869573937397));
#16914=CARTESIAN_POINT('Ctrl Pts',(-0.0650756559739905,0.160274727038081,
0.356634729011275));
#16915=CARTESIAN_POINT('Ctrl Pts',(-0.169951541620772,0.0322382168908211,
0.364573718648582));
#16916=CARTESIAN_POINT('Ctrl Pts',(-0.119248438453561,-0.125310171390688,
0.372512708285886));
#16917=CARTESIAN_POINT('Ctrl Pts',(0.0406184374886585,-0.168145685830938,
0.380451697923193));
#16918=CARTESIAN_POINT('Ctrl Pts',(0.163301917673335,-0.0570553486694088,
0.388390687560498));
#16919=CARTESIAN_POINT('Ctrl Pts',(0.136493684039406,0.106265249940549,
0.396329677197804));
#16920=CARTESIAN_POINT('Ctrl Pts',(-0.0152651628095069,0.172307295063139,
0.404268666835109));
#16921=CARTESIAN_POINT('Ctrl Pts',(-0.153049799296248,0.0806138205455782,
0.412207656472416));
#16922=CARTESIAN_POINT('Ctrl Pts',(-0.150727833715048,-0.0848760818555219,
0.420146646109721));
#16923=CARTESIAN_POINT('Ctrl Pts',(-0.0104248664208018,-0.172667748255674,
0.428085635747027));
#16924=CARTESIAN_POINT('Ctrl Pts',(0.139421351618932,-0.10239392482138,
0.436024625384332));
#16925=CARTESIAN_POINT('Ctrl Pts',(0.16163687742079,0.0616145192729195,
0.443963615021638));
#16926=CARTESIAN_POINT('Ctrl Pts',(0.0358849196425865,0.169219093691645,
0.451902604658944));
#16927=CARTESIAN_POINT('Ctrl Pts',(-0.122717222714247,0.121915185177559,
0.45984159429625));
#16928=CARTESIAN_POINT('Ctrl Pts',(-0.168980158036723,-0.0369937199732681,
0.467780583933555));
#16929=CARTESIAN_POINT('Ctrl Pts',(-0.0605533396431397,-0.162037409833775,
0.475719573570861));
#16930=CARTESIAN_POINT('Ctrl Pts',(0.103305911202344,-0.138746956140414,
0.483658563208167));
#16931=CARTESIAN_POINT('Ctrl Pts',(0.172595680358559,0.0115568269495825,
0.491597552845473));
#16932=CARTESIAN_POINT('Ctrl Pts',(0.0838859329010004,0.151281127008313,
0.499536542482778));
#16933=CARTESIAN_POINT('Ctrl Pts',(-0.0816156370489812,0.152517923263679,
0.507475532120084));
#16934=CARTESIAN_POINT('Ctrl Pts',(-0.172403684765527,0.0141350135070757,
0.51541452175739));
#16935=CARTESIAN_POINT('Ctrl Pts',(-0.105367974675403,-0.137187532379513,
0.523353511394695));
#16936=CARTESIAN_POINT('Ctrl Pts',(0.0581248948911363,-0.162924294448283,
0.531292501032001));
#16937=CARTESIAN_POINT('Ctrl Pts',(0.168408406744046,-0.039515030880773,
0.539231490669306));
#16938=CARTESIAN_POINT('Ctrl Pts',(0.124525564004667,0.120067535316156,
0.547170480306613));
#16939=CARTESIAN_POINT('Ctrl Pts',(-0.0333518982867267,0.169736501696743,
0.555109469943918));
#16940=CARTESIAN_POINT('Ctrl Pts',(-0.160697983451488,0.0640233335761385,
0.563048459581225));
#16941=CARTESIAN_POINT('Ctrl Pts',(-0.14093607811848,-0.100298808627811,
0.570987449218529));
#16942=CARTESIAN_POINT('Ctrl Pts',(0.00784314775175556,-0.172804265459278,
0.578926438855836));
#16943=CARTESIAN_POINT('Ctrl Pts',(0.149442509381278,-0.0871192603125336,
0.586865428493141));
#16944=CARTESIAN_POINT('Ctrl Pts',(0.154237495636292,0.0783174569774929,
0.594804418130446));
#16945=CARTESIAN_POINT('Ctrl Pts',(0.0178386252221998,0.172059909850489,
0.602743407767753));
#16946=CARTESIAN_POINT('Ctrl Pts',(-0.134890284021987,0.108293307291099,
0.610682397405058));
#16947=CARTESIAN_POINT('Ctrl Pts',(-0.164136382878957,-0.0546083962682395,
0.618621387042364));
#16948=CARTESIAN_POINT('Ctrl Pts',(-0.0431268722112106,-0.167519855601819,
0.62656037667967));
#16949=CARTESIAN_POINT('Ctrl Pts',(0.117362334288317,-0.127078368017432,
0.634499366316975));
#16950=CARTESIAN_POINT('Ctrl Pts',(0.170414367112955,0.0296946562375699,
0.642438355954282));
#16951=CARTESIAN_POINT('Ctrl Pts',(0.0674637261050104,0.159284257814778,
0.650377345591586));
#16952=CARTESIAN_POINT('Ctrl Pts',(-0.0972453325609638,0.143060037825677,
0.658316335228894));
#16953=CARTESIAN_POINT('Ctrl Pts',(-0.172932953925271,-0.00412584224812367,
0.666255324866198));
#16954=CARTESIAN_POINT('Ctrl Pts',(-0.0903123078403481,-0.147534796506203,
0.674194314503505));
#16955=CARTESIAN_POINT('Ctrl Pts',(0.0749830665657334,-0.155885755782802,
0.68213330414081));
#16956=CARTESIAN_POINT('Ctrl Pts',(0.17163658245605,-0.021533989188811,
0.690072293778116));
#16957=CARTESIAN_POINT('Ctrl Pts',(0.11116857013107,0.132530668686874,0.698011283415421));
#16958=CARTESIAN_POINT('Ctrl Pts',(-0.0510666492692211,0.165272582299639,
0.705950273052727));
#16959=CARTESIAN_POINT('Ctrl Pts',(-0.166553851089581,0.0467187736868841,
0.713889262690032));
#16960=CARTESIAN_POINT('Ctrl Pts',(-0.129572416918314,-0.114602870389546,
0.721828252327339));
#16961=CARTESIAN_POINT('Ctrl Pts',(0.0260236847639906,-0.171013440871999,
0.729767241964644));
#16962=CARTESIAN_POINT('Ctrl Pts',(0.157796886564457,-0.0708729265526718,
0.73770623160195));
#16963=CARTESIAN_POINT('Ctrl Pts',(0.145117853242075,0.0941468947867542,
0.745645221239255));
#16964=CARTESIAN_POINT('Ctrl Pts',(-0.000406629147419015,0.172981686256994,
0.753584210876562));
#16965=CARTESIAN_POINT('Ctrl Pts',(-0.145558870420566,0.0934635991681543,
0.761523200513868));
#16966=CARTESIAN_POINT('Ctrl Pts',(-0.157461941624574,-0.0716140074803496,
0.769462190151172));
#16967=CARTESIAN_POINT('Ctrl Pts',(-0.0252193968429213,-0.17113389830906,
0.777401179788479));
#16968=CARTESIAN_POINT('Ctrl Pts',(0.130109777350283,-0.113992433807847,
0.785340169425784));
#16969=CARTESIAN_POINT('Ctrl Pts',(0.166332367384696,0.0475012914327479,
0.793279159063091));
#16970=CARTESIAN_POINT('Ctrl Pts',(0.0502890745800368,0.165510839842773,
0.801218148700395));
#16971=CARTESIAN_POINT('Ctrl Pts',(-0.111790419467279,0.132006557575396,
0.809157138337702));
#16972=CARTESIAN_POINT('Ctrl Pts',(-0.171533445990104,-0.0223406811520247,
0.817096127975007));
#16973=CARTESIAN_POINT('Ctrl Pts',(-0.0742493586638003,-0.156236557391639,
0.825035117612313));
#16974=CARTESIAN_POINT('Ctrl Pts',(0.0910049278783345,-0.147108572929777,
0.832974107249618));
#16975=CARTESIAN_POINT('Ctrl Pts',(0.172950439922886,-0.00331277195964383,
0.840913096886925));
#16976=CARTESIAN_POINT('Ctrl Pts',(0.0965716772857839,0.143515644700454,
0.848852086524229));
#16977=CARTESIAN_POINT('Ctrl Pts',(-0.0682118374171683,0.158965324406771,
0.856791076161536));
#16978=CARTESIAN_POINT('Ctrl Pts',(-0.170552089827228,0.0288931442238776,
0.864730065798841));
#16979=CARTESIAN_POINT('Ctrl Pts',(-0.116763592698541,-0.127628729319482,
0.872669055436147));
#16980=CARTESIAN_POINT('Ctrl Pts',(0.0439139712140358,-0.167315248138923,
0.880608045073453));
#16981=CARTESIAN_POINT('Ctrl Pts',(0.164391304101163,-0.0538361241500125,
0.888547034710759));
#16982=CARTESIAN_POINT('Ctrl Pts',(0.134379664555536,0.108926281867684,
0.896486024348063));
#16983=CARTESIAN_POINT('Ctrl Pts',(-0.018647348250808,0.17197414204115,
0.904425013985371));
#16984=CARTESIAN_POINT('Ctrl Pts',(-0.154603991719776,0.0775914613336281,
0.912364003622676));
#16985=CARTESIAN_POINT('Ctrl Pts',(-0.149031276472826,-0.0878208845346985,
0.920302993259982));
#16986=CARTESIAN_POINT('Ctrl Pts',(-0.00703064139541984,-0.172839229369798,
0.928241982897287));
#16987=CARTESIAN_POINT('Ctrl Pts',(0.141406064038169,-0.099635105162837,
0.936180972534593));
#16988=CARTESIAN_POINT('Ctrl Pts',(0.160395209035295,0.064778129380991,
0.944119962171899));
#16989=CARTESIAN_POINT('Ctrl Pts',(0.03255353276219,0.169891426011666,0.952058951809204));
#16990=CARTESIAN_POINT('Ctrl Pts',(-0.125088671715395,0.119480765548496,
0.959997941446511));
#16991=CARTESIAN_POINT('Ctrl Pts',(-0.168220770124088,-0.040306347222682,
0.967936931083815));
#16992=CARTESIAN_POINT('Ctrl Pts',(-0.0573582824064844,-0.163195761485875,
0.975875920721122));
#16993=CARTESIAN_POINT('Ctrl Pts',(0.106011781834435,-0.136690640644722,
0.983814910358427));
#16994=CARTESIAN_POINT('Ctrl Pts',(0.17233532526783,0.014945393685262,0.991753899995733));
#16995=CARTESIAN_POINT('Ctrl Pts',(0.0808976893297158,0.152899944371113,
0.999692889633039));
#16996=CARTESIAN_POINT('Ctrl Pts',(-0.0845962369090198,0.150885074902754,
1.00763187927034));
#16997=CARTESIAN_POINT('Ctrl Pts',(-0.172648106016301,0.0107452601904448,
1.01557086890765));
#16998=CARTESIAN_POINT('Ctrl Pts',(-0.102652466413112,-0.13923110380544,
1.02350985854496));
#16999=CARTESIAN_POINT('Ctrl Pts',(0.0613144709582997,-0.161750934398167,
1.03144884818226));
#17000=CARTESIAN_POINT('Ctrl Pts',(0.169152212322519,-0.0361988700648799,
1.03938783781957));
#17001=CARTESIAN_POINT('Ctrl Pts',(0.122142696063681,0.12249077894222,1.04732682745687));
#17002=CARTESIAN_POINT('Ctrl Pts',(-0.0366800874558037,0.169048514669047,
1.05526581709418));
#17003=CARTESIAN_POINT('Ctrl Pts',(-0.161924764760067,0.0608539208677085,
1.06320480673148));
#17004=CARTESIAN_POINT('Ctrl Pts',(-0.138938417355371,-0.103048266896446,
1.07114379636879));
#17005=CARTESIAN_POINT('Ctrl Pts',(0.011236529066559,-0.172616828675865,
1.0790827860061));
#17006=CARTESIAN_POINT('Ctrl Pts',(0.151125203217684,-0.0841665140064042,
1.0870217756434));
#17007=CARTESIAN_POINT('Ctrl Pts',(0.152669111109608,0.0813324759279986,
1.09496076528071));
#17008=CARTESIAN_POINT('Ctrl Pts',(0.0144549108781955,0.172377158228925,
1.10289975491801));
#17009=CARTESIAN_POINT('Ctrl Pts',(-0.136991769602464,0.10562236594946,
1.11083874455532));
#17010=CARTESIAN_POINT('Ctrl Pts',(-0.163031873671196,-0.0578224635832477,
1.11877773419263));
#17011=CARTESIAN_POINT('Ctrl Pts',(-0.0398274706979539,-0.168334790537727,
1.12671672382993));
#17012=CARTESIAN_POINT('Ctrl Pts',(0.119836252144435,-0.124748153491552,
1.13465571346724));
#17013=CARTESIAN_POINT('Ctrl Pts',(0.169798099063322,0.0330368685268242,
1.14259470310454));
#17014=CARTESIAN_POINT('Ctrl Pts',(0.0643214233134591,0.160578901573361,
1.15053369274185));
#17015=CARTESIAN_POINT('Ctrl Pts',(-0.100037107244844,0.141121955420339,
1.15847268237915));
#17016=CARTESIAN_POINT('Ctrl Pts',(-0.172818522111203,-0.00752246920075927,
1.16641167201646));
#17017=CARTESIAN_POINT('Ctrl Pts',(-0.0873964240115842,-0.149280588817046,
1.17435066165376));
#17018=CARTESIAN_POINT('Ctrl Pts',(0.0780311106025284,-0.154382560238235,
1.18228965129107));
#17019=CARTESIAN_POINT('Ctrl Pts',(0.172026511281289,-0.01815787828917,
1.19022864092837));
#17020=CARTESIAN_POINT('Ctrl Pts',(0.10854343062882,0.134689096792963,1.19816763056568));
#17021=CARTESIAN_POINT('Ctrl Pts',(-0.0543037217972188,0.164237434607784,
1.20610662020299));
#17022=CARTESIAN_POINT('Ctrl Pts',(-0.167439538594998,0.0434376569656869,
1.21404560984029));
#17023=CARTESIAN_POINT('Ctrl Pts',(-0.127295933190098,-0.117126318651471,
1.2219845994776));
#17024=CARTESIAN_POINT('Ctrl Pts',(0.0293783748903316,-0.170469176734012,
1.2299235891149));
#17025=CARTESIAN_POINT('Ctrl Pts',(0.159158794190081,-0.0677591865323411,
1.23786257875221));
#17026=CARTESIAN_POINT('Ctrl Pts',(0.143240245273553,0.0969796950995427,
1.24580156838952));
#17027=CARTESIAN_POINT('Ctrl Pts',(-0.00380493129617075,0.172940312320012,
1.25374055802682));
#17028=CARTESIAN_POINT('Ctrl Pts',(-0.147366954032488,0.0905859259858403,
1.26167954766413));
#17029=CARTESIAN_POINT('Ctrl Pts',(-0.156024630070406,-0.074693667330688,
1.26961853730143));
#17030=CARTESIAN_POINT('Ctrl Pts',(-0.0218524503424686,-0.171596327294885,
1.27755752693874));
#17031=CARTESIAN_POINT('Ctrl Pts',(0.132324150022753,-0.111414309889572,
1.28549651657604));
#17032=CARTESIAN_POINT('Ctrl Pts',(0.165367059817933,0.0507598725070622,
1.29343550621335));
#17033=CARTESIAN_POINT('Ctrl Pts',(0.0470277596764783,0.166466870408131,
1.30137449585065));
#17034=CARTESIAN_POINT('Ctrl Pts',(-0.114362231391601,0.129784857201791,
1.30931348548797));
#17035=CARTESIAN_POINT('Ctrl Pts',(-0.171061437441431,-0.0257062980954763,
1.31725247512526));
#17036=CARTESIAN_POINT('Ctrl Pts',(-0.071165620995849,-0.157665099140374,
1.32519146476257));
#17037=CARTESIAN_POINT('Ctrl Pts',(0.0938774439379855,-0.145292307632914,
1.33313045439988));
#17038=CARTESIAN_POINT('Ctrl Pts',(0.172982143233999,8.56343898915854E-5,
1.34106944403719));
#17039=CARTESIAN_POINT('Ctrl Pts',(0.0937335447930804,0.145385183220099,
1.34900843367449));
#17040=CARTESIAN_POINT('Ctrl Pts',(-0.0713216883190155,0.157594562185848,
1.3569474233118));
#17041=CARTESIAN_POINT('Ctrl Pts',(-0.171086806821499,0.0255369173285507,
1.3648864129491));
#17042=CARTESIAN_POINT('Ctrl Pts',(-0.114233673229396,-0.129898019862958,
1.37282540258641));
#17043=CARTESIAN_POINT('Ctrl Pts',(0.0471925482590101,-0.166420232464351,
1.38076439222371));
#17044=CARTESIAN_POINT('Ctrl Pts',(0.165417247017141,-0.0505961085897048,
1.38870338186102));
#17045=CARTESIAN_POINT('Ctrl Pts',(0.132213753266125,0.111545248710567,
1.39664237149832));
#17046=CARTESIAN_POINT('Ctrl Pts',(-0.0220222951247444,0.17157464463752,
1.40458136113563));
#17047=CARTESIAN_POINT('Ctrl Pts',(-0.156098584526576,0.0745390809398717,
1.41252035077293));
#17048=CARTESIAN_POINT('Ctrl Pts',(-0.147277046608992,-0.0907316537045687,
1.42045934041024));
#17049=CARTESIAN_POINT('Ctrl Pts',(-0.00363398118293899,-0.172944250658386,
1.42839833004755));
#17050=CARTESIAN_POINT('Ctrl Pts',(0.143336722904634,-0.0968373407211472,
1.43633731968485));
#17051=CARTESIAN_POINT('Ctrl Pts',(0.159090624036536,0.0679158129692223,
1.44427630932216));
#17052=CARTESIAN_POINT('Ctrl Pts',(0.0292114869387437,0.170499931406899,
1.45221529895946));
#17053=CARTESIAN_POINT('Ctrl Pts',(-0.127415456569397,0.116996902323752,
1.46015428859677));
#17054=CARTESIAN_POINT('Ctrl Pts',(-0.167389576437263,-0.0435971050111283,
1.46809327823408));
#17055=CARTESIAN_POINT('Ctrl Pts',(-0.0541541359620402,-0.164303103757731,
1.47603226787138));
#17056=CARTESIAN_POINT('Ctrl Pts',(0.108701533888403,-0.13455879509903,
1.48397125750869));
#17057=CARTESIAN_POINT('Ctrl Pts',(0.171961157005542,0.0182848320604298,
1.49191024714599));
#17058=CARTESIAN_POINT('Ctrl Pts',(0.0779697431325927,0.154543202561513,
1.4998492367833));
#17059=CARTESIAN_POINT('Ctrl Pts',(-0.0877325682749983,0.149025855561406,
1.5077882264206));
#17060=CARTESIAN_POINT('Ctrl Pts',(-0.144149484752264,0.0548439265155397,
1.51308088617881));
#17061=CARTESIAN_POINT('Ctrl Pts',(-0.146217781693078,0.00621955116994065,
1.51572721605791));
#17062=CARTESIAN_POINT('Ctrl Pts',(0.0795408277542855,-0.111329858282327,
-0.0109985226280624));
#17063=CARTESIAN_POINT('Ctrl Pts',(0.116563307192903,-0.0848787452970238,
-0.00835219274896048));
#17064=CARTESIAN_POINT('Ctrl Pts',(0.16150817751539,0.00739908052493189,
-0.00305953299075667));
#17065=CARTESIAN_POINT('Ctrl Pts',(0.0812084309002137,0.139981433724326,
0.00487945664654907));
#17066=CARTESIAN_POINT('Ctrl Pts',(-0.0734975292821143,0.144003850402812,
0.0128184462838548));
#17067=CARTESIAN_POINT('Ctrl Pts',(-0.160887120581772,0.0164101388376342,
0.0207574359211605));
#17068=CARTESIAN_POINT('Ctrl Pts',(-0.101013704785435,-0.126315124179183,
0.0286964255584662));
#17069=CARTESIAN_POINT('Ctrl Pts',(0.0513403816191153,-0.153350170642076,
0.0366354151957719));
#17070=CARTESIAN_POINT('Ctrl Pts',(0.156690838735662,-0.0400338514845966,
0.0445744048330777));
#17071=CARTESIAN_POINT('Ctrl Pts',(0.118604220350264,0.109946623274354,
0.0525133944703833));
#17072=CARTESIAN_POINT('Ctrl Pts',(-0.0280578283917351,0.15927012049393,
0.0604523841076892));
#17073=CARTESIAN_POINT('Ctrl Pts',(-0.14903412333264,0.0627971513379326,
0.0683913737449947));
#17074=CARTESIAN_POINT('Ctrl Pts',(-0.133580279395553,-0.0911646307683348,
0.0763303633823007));
#17075=CARTESIAN_POINT('Ctrl Pts',(0.0041573593468571,-0.161670216863261,
0.0842693530196062));
#17076=CARTESIAN_POINT('Ctrl Pts',(0.138089113144455,-0.0841784443595545,
0.0922083426569122));
#17077=CARTESIAN_POINT('Ctrl Pts',(0.14560980428584,0.0703732645446943,
0.100147332294218));
#17078=CARTESIAN_POINT('Ctrl Pts',(0.0198346691022095,0.160502893816501,
0.108086321931524));
#17079=CARTESIAN_POINT('Ctrl Pts',(-0.124097730593135,0.103703218031488,
0.116025311568829));
#17080=CARTESIAN_POINT('Ctrl Pts',(-0.154427171169137,-0.0480296962598115,
0.123964301206135));
#17081=CARTESIAN_POINT('Ctrl Pts',(-0.0433891157712434,-0.155794689166463,
0.13190329084344));
#17082=CARTESIAN_POINT('Ctrl Pts',(0.107368699171666,-0.12094033522185,
0.139842280480747));
#17083=CARTESIAN_POINT('Ctrl Pts',(0.15983782968835,0.0246266142906177,
0.147781270118052));
#17084=CARTESIAN_POINT('Ctrl Pts',(0.0659863808909888,0.147649582370873,
0.155720259755358));
#17085=CARTESIAN_POINT('Ctrl Pts',(-0.0882710769349216,0.135509478890084,
0.163659249392663));
#17086=CARTESIAN_POINT('Ctrl Pts',(-0.161722413615419,-0.00068026650363694,
0.171598239029969));
#17087=CARTESIAN_POINT('Ctrl Pts',(-0.0871279640988751,-0.136247273976568,
0.179537228667275));
#17088=CARTESIAN_POINT('Ctrl Pts',(0.0672261652318651,-0.147089240053593,
0.187476218304581));
#17089=CARTESIAN_POINT('Ctrl Pts',(0.160039347628626,-0.023281087390596,
0.195415207941886));
#17090=CARTESIAN_POINT('Ctrl Pts',(0.106347475470598,0.121839305139765,
0.203354197579192));
#17091=CARTESIAN_POINT('Ctrl Pts',(-0.0446982220051161,0.15542416405057,
0.211293187216498));
#17092=CARTESIAN_POINT('Ctrl Pts',(-0.154825760608133,0.0467288526640558,
0.219232176853804));
#17093=CARTESIAN_POINT('Ctrl Pts',(-0.12322092627477,-0.104743520787053,
0.227171166491109));
#17094=CARTESIAN_POINT('Ctrl Pts',(0.0211842211805034,-0.160330379506191,
0.235110156128415));
#17095=CARTESIAN_POINT('Ctrl Pts',(0.146196665995071,-0.0691457639426259,
0.24304914576572));
#17096=CARTESIAN_POINT('Ctrl Pts',(0.137376082602736,0.0853370596399817,
0.250988135403027));
#17097=CARTESIAN_POINT('Ctrl Pts',(0.00279711058556459,0.161699653653757,
0.258927125040332));
#17098=CARTESIAN_POINT('Ctrl Pts',(-0.134342424474264,0.0900372967480426,
0.266866114677638));
#17099=CARTESIAN_POINT('Ctrl Pts',(-0.148500677015507,-0.0640480346713102,
0.274805104314944));
#17100=CARTESIAN_POINT('Ctrl Pts',(-0.0267167371651392,-0.159501779847699,
0.282744093952249));
#17101=CARTESIAN_POINT('Ctrl Pts',(0.119524544542348,-0.108942576944327,
0.290683083589556));
#17102=CARTESIAN_POINT('Ctrl Pts',(0.156349297273321,0.0413460888291301,
0.29862207322686));
#17103=CARTESIAN_POINT('Ctrl Pts',(0.0500469836677093,0.153785243912065,
0.306561062864167));
#17104=CARTESIAN_POINT('Ctrl Pts',(-0.102069913541897,0.125444547784578,
0.314500052501472));
#17105=CARTESIAN_POINT('Ctrl Pts',(-0.160748800211922,-0.0177320345633525,
0.322439042138778));
#17106=CARTESIAN_POINT('Ctrl Pts',(-0.0722731771226978,-0.144676154524232,
0.330378031776084));
#17107=CARTESIAN_POINT('Ctrl Pts',(0.082363586418043,-0.139179170322594,
0.338317021413389));
#17108=CARTESIAN_POINT('Ctrl Pts',(0.16160213133829,-0.00627319426210969,
0.346256011050695));
#17109=CARTESIAN_POINT('Ctrl Pts',(0.0929050003357002,0.132375461215256,
0.354195000688001));
#17110=CARTESIAN_POINT('Ctrl Pts',(-0.0608402912787218,0.149843454232904,
0.362133990325306));
#17111=CARTESIAN_POINT('Ctrl Pts',(-0.158890465884947,0.0301400343429239,
0.370072979962613));
#17112=CARTESIAN_POINT('Ctrl Pts',(-0.1114873084483,-0.117154521356547,
0.378011969599918));
#17113=CARTESIAN_POINT('Ctrl Pts',(0.0379748391485164,-0.157202141877815,
0.385950959237223));
#17114=CARTESIAN_POINT('Ctrl Pts',(0.152673624090564,-0.0533419752763387,
0.39388994887453));
#17115=CARTESIAN_POINT('Ctrl Pts',(0.127610169584502,0.0993491139263089,
0.401828938511835));
#17116=CARTESIAN_POINT('Ctrl Pts',(-0.014271649480085,0.16109289816887,
0.409767928149142));
#17117=CARTESIAN_POINT('Ctrl Pts',(-0.143088751545671,0.0753671745551693,
0.417706917786446));
#17118=CARTESIAN_POINT('Ctrl Pts',(-0.140917908083783,-0.0793520321139836,
0.425645907423752));
#17119=CARTESIAN_POINT('Ctrl Pts',(-0.00974637750615997,-0.161429891732714,
0.433584897061058));
#17120=CARTESIAN_POINT('Ctrl Pts',(0.130347293715478,-0.0957297489831606,
0.441523886698364));
#17121=CARTESIAN_POINT('Ctrl Pts',(0.15111695082405,0.0576044181723055,
0.449462876335669));
#17122=CARTESIAN_POINT('Ctrl Pts',(0.0335493961742207,0.158205688379633,
0.457401865972975));
#17123=CARTESIAN_POINT('Ctrl Pts',(-0.114730331382826,0.113980493419335,
0.465340855610281));
#17124=CARTESIAN_POINT('Ctrl Pts',(-0.157982303542021,-0.03458603167299,
0.473279845247587));
#17125=CARTESIAN_POINT('Ctrl Pts',(-0.0566123040428622,-0.151491415104245,
0.481218834884892));
#17126=CARTESIAN_POINT('Ctrl Pts',(0.0965823799129518,-0.129716790392294,
0.489157824522198));
#17127=CARTESIAN_POINT('Ctrl Pts',(0.161362514281243,0.0108046658515635,
0.497096814159504));
#17128=CARTESIAN_POINT('Ctrl Pts',(0.0784263257203939,0.141435191000425,
0.50503580379681));
#17129=CARTESIAN_POINT('Ctrl Pts',(-0.076303789130349,0.14259149197508,
0.512974793434115));
#17130=CARTESIAN_POINT('Ctrl Pts',(-0.161183014472451,0.0132150544797126,
0.520913783071421));
#17131=CARTESIAN_POINT('Ctrl Pts',(-0.0985102366584373,-0.128258859705,
0.528852772708727));
#17132=CARTESIAN_POINT('Ctrl Pts',(0.0543419114689404,-0.152320577983508,
0.536791762346032));
#17133=CARTESIAN_POINT('Ctrl Pts',(0.157447763940923,-0.0369432463290883,
0.544730751983338));
#17134=CARTESIAN_POINT('Ctrl Pts',(0.116420979124965,0.112253095453589,
0.552669741620643));
#17135=CARTESIAN_POINT('Ctrl Pts',(-0.0311812332291155,0.158689421555565,
0.56060873125795));
#17136=CARTESIAN_POINT('Ctrl Pts',(-0.150239163551416,0.0598564579197502,
0.568547720895255));
#17137=CARTESIAN_POINT('Ctrl Pts',(-0.131763436204723,-0.0937709907106254,
0.576486710532561));
#17138=CARTESIAN_POINT('Ctrl Pts',(0.00733268664935855,-0.161557523891122,
0.584425700169866));
#17139=CARTESIAN_POINT('Ctrl Pts',(0.139716237417787,-0.0814492162095161,
0.592364689807173));
#17140=CARTESIAN_POINT('Ctrl Pts',(0.144199148209332,0.0732202668325601,
0.600303679444478));
#17141=CARTESIAN_POINT('Ctrl Pts',(0.0166776214282734,0.160861613702037,
0.608242669081784));
#17142=CARTESIAN_POINT('Ctrl Pts',(-0.126111124778327,0.101245177793678,
0.616181658719089));
#17143=CARTESIAN_POINT('Ctrl Pts',(-0.153453779210204,-0.0510542795996006,
0.624120648356396));
#17144=CARTESIAN_POINT('Ctrl Pts',(-0.0403200156494649,-0.156617042997737,
0.6320596379937));
#17145=CARTESIAN_POINT('Ctrl Pts',(0.10972395892722,-0.118807637198397,
0.639998627631007));
#17146=CARTESIAN_POINT('Ctrl Pts',(0.159323168980049,0.0277620180369333,
0.647937617268312));
#17147=CARTESIAN_POINT('Ctrl Pts',(0.0630729369615192,0.148917448414806,
0.655876606905618));
#17148=CARTESIAN_POINT('Ctrl Pts',(-0.0909162461746061,0.133749160748195,
0.663815596542924));
#17149=CARTESIAN_POINT('Ctrl Pts',(-0.161677836835157,-0.00385731715476066,
0.671754586180229));
#17150=CARTESIAN_POINT('Ctrl Pts',(-0.0844344483789265,-0.137932685561743,
0.679693575817536));
#17151=CARTESIAN_POINT('Ctrl Pts',(0.0701028908975481,-0.145740133481257,
0.687632565454841));
#17152=CARTESIAN_POINT('Ctrl Pts',(0.1604658380222,-0.0201324774223393,
0.695571555092147));
#17153=CARTESIAN_POINT('Ctrl Pts',(0.10393330787963,0.123905081947942,0.703510544729453));
#17154=CARTESIAN_POINT('Ctrl Pts',(-0.0477430426119635,0.15451603056473,
0.711449534366758));
#17155=CARTESIAN_POINT('Ctrl Pts',(-0.155713909636705,0.0436781428746717,
0.719388524004064));
#17156=CARTESIAN_POINT('Ctrl Pts',(-0.121139364160222,-0.10714409115852,
0.72732751364137));
#17157=CARTESIAN_POINT('Ctrl Pts',(0.0243299669821161,-0.159883252800214,
0.735266503278675));
#17158=CARTESIAN_POINT('Ctrl Pts',(0.147526880793862,-0.0662602540182413,
0.743205492915981));
#17159=CARTESIAN_POINT('Ctrl Pts',(0.135673045916277,0.0880194662056535,
0.751144482553287));
#17160=CARTESIAN_POINT('Ctrl Pts',(-0.000380164216571841,0.161723397486253,
0.759083472190592));
#17161=CARTESIAN_POINT('Ctrl Pts',(-0.136085360063504,0.0873806419964673,
0.767022461827899));
#17162=CARTESIAN_POINT('Ctrl Pts',(-0.147213735311121,-0.0669531026545853,
0.774961451465203));
#17163=CARTESIAN_POINT('Ctrl Pts',(-0.023578025097595,-0.159995870421162,
0.78290044110251));
#17164=CARTESIAN_POINT('Ctrl Pts',(0.121641751185188,-0.106573384050283,
0.790839430739816));
#17165=CARTESIAN_POINT('Ctrl Pts',(0.155506840911589,0.0444097314676148,
0.798778420377121));
#17166=CARTESIAN_POINT('Ctrl Pts',(0.047016075363265,0.15473878142458,0.806717410014428));
#17167=CARTESIAN_POINT('Ctrl Pts',(-0.104514684958047,0.123415081928621,
0.814656399651731));
#17168=CARTESIAN_POINT('Ctrl Pts',(-0.16036941405942,-0.020886666885039,
0.82259538928904));
#17169=CARTESIAN_POINT('Ctrl Pts',(-0.0694169354231278,-0.146068103622213,
0.830534378926343));
#17170=CARTESIAN_POINT('Ctrl Pts',(0.085081990139753,-0.137534202194171,
0.838473368563651));
#17171=CARTESIAN_POINT('Ctrl Pts',(0.161694184779289,-0.00309716449182502,
0.846412358200955));
#17172=CARTESIAN_POINT('Ctrl Pts',(0.0902864348795877,0.134175115040242,
0.854351347838261));
#17173=CARTESIAN_POINT('Ctrl Pts',(-0.0637723584188847,0.148619272374149,
0.862290337475567));
#17174=CARTESIAN_POINT('Ctrl Pts',(-0.159451928190027,0.0270126713934565,
0.870229327112872));
#17175=CARTESIAN_POINT('Ctrl Pts',(-0.109164185657521,-0.119322178948671,
0.878168316750179));
#17176=CARTESIAN_POINT('Ctrl Pts',(0.0410558873341998,-0.156425752146281,
0.886107306387484));
#17177=CARTESIAN_POINT('Ctrl Pts',(0.153692109215179,-0.0503322698109037,
0.894046296024789));
#17178=CARTESIAN_POINT('Ctrl Pts',(0.125633738317809,0.101836956040625,
0.901985285662096));
#17179=CARTESIAN_POINT('Ctrl Pts',(-0.0174337097671096,0.160781427979367,
0.909924275299401));
#17180=CARTESIAN_POINT('Ctrl Pts',(-0.144541791370401,0.072541521673891,
0.917863264936708));
#17181=CARTESIAN_POINT('Ctrl Pts',(-0.13933176907,-0.082105176128868,0.925802254574012));
#17182=CARTESIAN_POINT('Ctrl Pts',(-0.00657306121577474,-0.161590212220858,
0.933741244211319));
#17183=CARTESIAN_POINT('Ctrl Pts',(0.132202833700187,-0.0931504835251481,
0.941680233848624));
#17184=CARTESIAN_POINT('Ctrl Pts',(0.149956094815541,0.0605621288182698,
0.949619223485929));
#17185=CARTESIAN_POINT('Ctrl Pts',(0.0304348282896272,0.158834262822317,
0.957558213123236));
#17186=CARTESIAN_POINT('Ctrl Pts',(-0.116947437700435,0.111704514835484,
0.965497202760542));
#17187=CARTESIAN_POINT('Ctrl Pts',(-0.157272339407096,-0.0376830608728604,
0.973436192397847));
#17188=CARTESIAN_POINT('Ctrl Pts',(-0.0536251929639052,-0.152574376940928,
0.981375182035153));
#17189=CARTESIAN_POINT('Ctrl Pts',(0.0991121424632477,-0.127794307524525,
0.989314171672459));
#17190=CARTESIAN_POINT('Ctrl Pts',(0.161119104064031,0.0139726921146952,
0.997253161309763));
#17191=CARTESIAN_POINT('Ctrl Pts',(0.0756325681075411,0.142948649734045,
1.00519215094707));
#17192=CARTESIAN_POINT('Ctrl Pts',(-0.0790904005129918,0.141064915432658,
1.01313114058437));
#17193=CARTESIAN_POINT('Ctrl Pts',(-0.161411527883023,0.0100459188627121,
1.02107013022168));
#17194=CARTESIAN_POINT('Ctrl Pts',(-0.095971463730607,-0.130169427934261,
1.02900911985899));
#17195=CARTESIAN_POINT('Ctrl Pts',(0.0573238981132153,-0.151223584550935,
1.03694810949629));
#17196=CARTESIAN_POINT('Ctrl Pts',(0.158143159897702,-0.0338429135403315,
1.0448870991336));
#17197=CARTESIAN_POINT('Ctrl Pts',(0.114193197054413,0.114518625410106,
1.0528260887709));
#17198=CARTESIAN_POINT('Ctrl Pts',(-0.0342928115212847,0.158046211271557,
1.06076507840821));
#17199=CARTESIAN_POINT('Ctrl Pts',(-0.151386101389109,0.0568933223281485,
1.06870406804552));
#17200=CARTESIAN_POINT('Ctrl Pts',(-0.129895790602315,-0.0963415040526547,
1.07664305768282));
#17201=CARTESIAN_POINT('Ctrl Pts',(0.0105052141409744,-0.161382286187737,
1.08458204732013));
#17202=CARTESIAN_POINT('Ctrl Pts',(0.141289415307547,-0.0786886455683398,
1.09252103695743));
#17203=CARTESIAN_POINT('Ctrl Pts',(0.14273283995608,0.076039057183793,1.10046002659474));
#17204=CARTESIAN_POINT('Ctrl Pts',(0.013514131745196,0.161158214381091,
1.10839901623204));
#17205=CARTESIAN_POINT('Ctrl Pts',(-0.128075837894479,0.0987480712062529,
1.11633800586935));
#17206=CARTESIAN_POINT('Ctrl Pts',(-0.152421155552179,-0.0540591635106084,
1.12427699550666));
#17207=CARTESIAN_POINT('Ctrl Pts',(-0.0372353514058616,-0.157378938949945,
1.13221598514396));
#17208=CARTESIAN_POINT('Ctrl Pts',(0.11203686504723,-0.116629081663695,
1.14015497478127));
#17209=CARTESIAN_POINT('Ctrl Pts',(0.158747009937404,0.0308867067726846,
1.14809396441857));
#17210=CARTESIAN_POINT('Ctrl Pts',(0.0601351468730053,0.150127831962932,
1.15603295405588));
#17211=CARTESIAN_POINT('Ctrl Pts',(-0.0935263218228598,0.13193721592339,
1.16397194369318));
#17212=CARTESIAN_POINT('Ctrl Pts',(-0.161570852667341,-0.00703287904607843,
1.17191093333049));
#17213=CARTESIAN_POINT('Ctrl Pts',(-0.0817083410685703,-0.13956485524354,
1.17984992296779));
#17214=CARTESIAN_POINT('Ctrl Pts',(0.0729525569401478,-0.144334771469742,
1.1877889126051));
#17215=CARTESIAN_POINT('Ctrl Pts',(0.160830388835411,-0.016976096323307,
1.19572790224241));
#17216=CARTESIAN_POINT('Ctrl Pts',(0.101479022178261,0.125923031559255,
1.20366689187971));
#17217=CARTESIAN_POINT('Ctrl Pts',(-0.0507694344715009,0.153548254118279,
1.21160588151702));
#17218=CARTESIAN_POINT('Ctrl Pts',(-0.15654195331917,0.0406105733811438,
1.21954487115432));
#17219=CARTESIAN_POINT('Ctrl Pts',(-0.119011042423884,-0.109503304062093,
1.22748386079163));
#17220=CARTESIAN_POINT('Ctrl Pts',(0.0274663214511058,-0.159374411387982,
1.23542285042894));
#17221=CARTESIAN_POINT('Ctrl Pts',(0.148800150427453,-0.0633491677300162,
1.24336184006624));
#17222=CARTESIAN_POINT('Ctrl Pts',(0.133917639627974,0.0906678973829495,
1.25130082970354));
#17223=CARTESIAN_POINT('Ctrl Pts',(-0.00355729227603857,0.161684716318317,
1.25923981934086));
#17224=CARTESIAN_POINT('Ctrl Pts',(-0.137775766897813,0.0846902584421788,
1.26717880897816));
#17225=CARTESIAN_POINT('Ctrl Pts',(-0.14586996931591,-0.0698323268364953,
1.27511779861547));
#17226=CARTESIAN_POINT('Ctrl Pts',(-0.0204302119447119,-0.160428202816007,
1.28305678825277));
#17227=CARTESIAN_POINT('Ctrl Pts',(0.123712004283314,-0.104163053984564,
1.29099577789008));
#17228=CARTESIAN_POINT('Ctrl Pts',(0.15460435913624,0.0474562320176185,
1.29893476752738));
#17229=CARTESIAN_POINT('Ctrl Pts',(0.043967018911749,0.155632589980133,
1.30687375716469));
#17230=CARTESIAN_POINT('Ctrl Pts',(-0.106919113837756,0.121337978043289,
1.31481274680199));
#17231=CARTESIAN_POINT('Ctrl Pts',(-0.159928125575155,-0.0240332370134145,
1.3227517364393));
#17232=CARTESIAN_POINT('Ctrl Pts',(-0.0665338988230771,-0.147403670583407,
1.33069072607661));
#17233=CARTESIAN_POINT('Ctrl Pts',(0.0877675522160205,-0.135836146169277,
1.33862971571391));
#17234=CARTESIAN_POINT('Ctrl Pts',(0.161723824721502,8.00609866524728E-5,
1.34656870535122));
#17235=CARTESIAN_POINT('Ctrl Pts',(0.0876330185603928,0.135922977069285,
1.35450769498852));
#17236=CARTESIAN_POINT('Ctrl Pts',(-0.0666798087068602,0.147337724435113,
1.36244668462583));
#17237=CARTESIAN_POINT('Ctrl Pts',(-0.159951843822013,0.0238748801740983,
1.37038567426313));
#17238=CARTESIAN_POINT('Ctrl Pts',(-0.106798922716859,-0.121443775659372,
1.37832466390044));
#17239=CARTESIAN_POINT('Ctrl Pts',(0.0441210824430389,-0.155588987406456,
1.38626365353774));
#17240=CARTESIAN_POINT('Ctrl Pts',(0.154651279966657,-0.0473031264624986,
1.39420264317505));
#17241=CARTESIAN_POINT('Ctrl Pts',(0.123608792556459,0.10428547082216,1.40214163281236));
#17242=CARTESIAN_POINT('Ctrl Pts',(-0.020589002599541,0.160407931346284,
1.41008062244966));
#17243=CARTESIAN_POINT('Ctrl Pts',(-0.145939110542184,0.0696878015005003,
1.41801961208697));
#17244=CARTESIAN_POINT('Ctrl Pts',(-0.137691710982408,-0.0848265016612731,
1.42595860172427));
#17245=CARTESIAN_POINT('Ctrl Pts',(-0.00339746822928561,-0.161688398335044,
1.43389759136158));
#17246=CARTESIAN_POINT('Ctrl Pts',(0.134007838137522,-0.0905348079547059,
1.44183658099889));
#17247=CARTESIAN_POINT('Ctrl Pts',(0.148736417039967,0.0634956003383226,
1.44977557063619));
#17248=CARTESIAN_POINT('Ctrl Pts',(0.0273102951854726,0.159403164432859,
1.4577145602735));
#17249=CARTESIAN_POINT('Ctrl Pts',(-0.119122786779006,0.109382310628272,
1.4656535499108));
#17250=CARTESIAN_POINT('Ctrl Pts',(-0.156495242883694,-0.0407596439572756,
1.47359253954811));
#17251=CARTESIAN_POINT('Ctrl Pts',(-0.0506295842364637,-0.153609649276743,
1.48153152918541));
#17252=CARTESIAN_POINT('Ctrl Pts',(0.10162683549218,-0.125801210382132,
1.48947051882272));
#17253=CARTESIAN_POINT('Ctrl Pts',(0.160769288057966,0.017094787472962,
1.49740950846002));
#17254=CARTESIAN_POINT('Ctrl Pts',(0.0728951834924312,0.144484958595688,
1.50534849809733));
#17255=CARTESIAN_POINT('Ctrl Pts',(-0.0820226078184241,0.139326700971572,
1.51328748773464));
#17256=CARTESIAN_POINT('Ctrl Pts',(-0.134767702434085,0.0512744806661359,
1.51858014749284));
#17257=CARTESIAN_POINT('Ctrl Pts',(-0.136701386950156,0.00581475974600206,
1.52122647737194));
#17258=CARTESIAN_POINT('Ctrl Pts',(0.0740036351041134,-0.103579689087085,
-0.0054992613140312));
#17259=CARTESIAN_POINT('Ctrl Pts',(0.108448814220036,-0.0789699563406641,
-0.00285293143492929));
#17260=CARTESIAN_POINT('Ctrl Pts',(0.150264871169078,0.00688399744800666,
0.00243972832327453));
#17261=CARTESIAN_POINT('Ctrl Pts',(0.0755551489391376,0.130236700260234,
0.0103787179605803));
#17262=CARTESIAN_POINT('Ctrl Pts',(-0.0683810376584167,0.133979098529349,
0.0183177075978859));
#17263=CARTESIAN_POINT('Ctrl Pts',(-0.14968704878538,0.0152677557027674,
0.0262566972351917));
#17264=CARTESIAN_POINT('Ctrl Pts',(-0.0939816891590436,-0.11752176362514,
0.0341956868724974));
#17265=CARTESIAN_POINT('Ctrl Pts',(0.0477663481097245,-0.142674779628989,
0.0421346765098031));
#17266=CARTESIAN_POINT('Ctrl Pts',(0.14578288888032,-0.0372469160898187,
0.0500736661471088));
#17267=CARTESIAN_POINT('Ctrl Pts',(0.110347650287512,0.102292747252513,
0.0580126557844146));
#17268=CARTESIAN_POINT('Ctrl Pts',(-0.0261045975097209,0.148182615303324,
0.0659516454217203));
#17269=CARTESIAN_POINT('Ctrl Pts',(-0.13865919166998,0.0584255608647477,
0.073890635059026));
#17270=CARTESIAN_POINT('Ctrl Pts',(-0.124281158904105,-0.0848182532198701,
0.0818296246963318));
#17271=CARTESIAN_POINT('Ctrl Pts',(0.00386794697500161,-0.15041563023346,
0.0897686143336374));
#17272=CARTESIAN_POINT('Ctrl Pts',(0.128476112576568,-0.0783184064825255,
0.0977076039709433));
#17273=CARTESIAN_POINT('Ctrl Pts',(0.135473254782295,0.0654742669580799,
0.105646593608249));
#17274=CARTESIAN_POINT('Ctrl Pts',(0.0184538891044151,0.149329569763132,
0.113585583245555));
#17275=CARTESIAN_POINT('Ctrl Pts',(-0.115458732720671,0.096483973363118,
0.12152457288286));
#17276=CARTESIAN_POINT('Ctrl Pts',(-0.143676805334049,-0.0446861343604874,
0.129463562520166));
#17277=CARTESIAN_POINT('Ctrl Pts',(-0.0403686054279526,-0.144949124289353,
0.137402552157472));
#17278=CARTESIAN_POINT('Ctrl Pts',(0.0998942839726139,-0.112521137758025,
0.145341541794778));
#17279=CARTESIAN_POINT('Ctrl Pts',(0.14871080372247,0.0229122455632766,
0.153280531432083));
#17280=CARTESIAN_POINT('Ctrl Pts',(0.0613927738894439,0.137371034794898,
0.161219521069389));
#17281=CARTESIAN_POINT('Ctrl Pts',(-0.0821261326059948,0.126076058196294,
0.169158510706695));
#17282=CARTESIAN_POINT('Ctrl Pts',(-0.150464193336327,-0.000632910110818063,
0.177097500344));
#17283=CARTESIAN_POINT('Ctrl Pts',(-0.0810625969653723,-0.126762492068094,
0.185036489981306));
#17284=CARTESIAN_POINT('Ctrl Pts',(0.0625462512992226,-0.136849700411639,
0.192975479618612));
#17285=CARTESIAN_POINT('Ctrl Pts',(0.148898293097928,-0.0216603868066741,
0.200914469255917));
#17286=CARTESIAN_POINT('Ctrl Pts',(0.0989441522193119,0.113357526360621,
0.208853458893223));
#17287=CARTESIAN_POINT('Ctrl Pts',(-0.0415865789238149,0.144604393083411,
0.216792448530529));
#17288=CARTESIAN_POINT('Ctrl Pts',(-0.144047647180085,0.0434758483035601,
0.224731438167835));
#17289=CARTESIAN_POINT('Ctrl Pts',(-0.114642966671137,-0.0974518559926297,
0.232670427805141));
#17290=CARTESIAN_POINT('Ctrl Pts',(0.0197094928286333,-0.149169064945282,
0.240609417442446));
#17291=CARTESIAN_POINT('Ctrl Pts',(0.136019262424063,-0.0643322181611298,
0.248548407079752));
#17292=CARTESIAN_POINT('Ctrl Pts',(0.127812719278849,0.0793963653730636,
0.256487396717058));
#17293=CARTESIAN_POINT('Ctrl Pts',(0.00260239121171357,0.150443017797356,
0.264426386354363));
#17294=CARTESIAN_POINT('Ctrl Pts',(-0.124990247656303,0.0837693979610897,
0.272365375991669));
#17295=CARTESIAN_POINT('Ctrl Pts',(-0.138162880936044,-0.0595893646165358,
0.280304365628975));
#17296=CARTESIAN_POINT('Ctrl Pts',(-0.0248568656394851,-0.148398147813718,
0.288243355266281));
#17297=CARTESIAN_POINT('Ctrl Pts',(0.111203906597776,-0.101358597076653,
0.296182344903586));
#17298=CARTESIAN_POINT('Ctrl Pts',(0.145465123646218,0.0384678027257296,
0.304121334540892));
#17299=CARTESIAN_POINT('Ctrl Pts',(0.0465629893725541,0.143079565503422,
0.312060324178198));
#17300=CARTESIAN_POINT('Ctrl Pts',(-0.0949643705016135,0.116711791945748,
0.319999313815503));
#17301=CARTESIAN_POINT('Ctrl Pts',(-0.149558357514911,-0.0164976283567656,
0.327938303452809));
#17302=CARTESIAN_POINT('Ctrl Pts',(-0.0672419181269484,-0.134604600554976,
0.335877293090115));
#17303=CARTESIAN_POINT('Ctrl Pts',(0.0766298889166206,-0.12949028600085,
0.343816282727421));
#17304=CARTESIAN_POINT('Ctrl Pts',(0.150352284446295,-0.00583648916182633,
0.351755272364726));
#17305=CARTESIAN_POINT('Ctrl Pts',(0.0864374678803939,0.123160213504125,
0.359694262002032));
#17306=CARTESIAN_POINT('Ctrl Pts',(-0.0566049265834532,0.139412181427728,
0.367633251639338));
#17307=CARTESIAN_POINT('Ctrl Pts',(-0.147829390149123,0.0280418517950267,
0.375572241276644));
#17308=CARTESIAN_POINT('Ctrl Pts',(-0.103726178443039,-0.108998871322406,
0.383511230913949));
#17309=CARTESIAN_POINT('Ctrl Pts',(0.0353312408083745,-0.146258597924691,
0.391450220551255));
#17310=CARTESIAN_POINT('Ctrl Pts',(0.142045330507792,-0.0496286018832686,
0.399389210188561));
#17311=CARTESIAN_POINT('Ctrl Pts',(0.118726655129599,0.0924329779120693,
0.407328199825866));
#17312=CARTESIAN_POINT('Ctrl Pts',(-0.0132781361506635,0.1498785012746,
0.415267189463172));
#17313=CARTESIAN_POINT('Ctrl Pts',(-0.133127703795094,0.0701205285647604,
0.423206179100478));
#17314=CARTESIAN_POINT('Ctrl Pts',(-0.131107982452518,-0.0738279823724454,
0.431145168737783));
#17315=CARTESIAN_POINT('Ctrl Pts',(-0.00906788859151817,-0.150192035209753,
0.439084158375089));
#17316=CARTESIAN_POINT('Ctrl Pts',(0.121273235812024,-0.0890655731449414,
0.447023148012395));
#17317=CARTESIAN_POINT('Ctrl Pts',(0.14059702422731,0.0535943170716914,
0.4549621376497));
#17318=CARTESIAN_POINT('Ctrl Pts',(0.031213872705855,0.14719228306762,0.462901127287006));
#17319=CARTESIAN_POINT('Ctrl Pts',(-0.106743440051405,0.106045801661112,
0.470840116924312));
#17320=CARTESIAN_POINT('Ctrl Pts',(-0.146984449047318,-0.0321783433727119,
0.478779106561618));
#17321=CARTESIAN_POINT('Ctrl Pts',(-0.0526712684425847,-0.140945420374714,
0.486718096198923));
#17322=CARTESIAN_POINT('Ctrl Pts',(0.0898588486235595,-0.120686624644175,
0.49465708583623));
#17323=CARTESIAN_POINT('Ctrl Pts',(0.150129348203927,0.0100525047535443,
0.502596075473534));
#17324=CARTESIAN_POINT('Ctrl Pts',(0.0729667185397875,0.131589254992538,
0.510535065110842));
#17325=CARTESIAN_POINT('Ctrl Pts',(-0.0709919412117167,0.132665060686482,
0.518474054748145));
#17326=CARTESIAN_POINT('Ctrl Pts',(-0.149962344179375,0.0122950954523496,
0.526413044385453));
#17327=CARTESIAN_POINT('Ctrl Pts',(-0.0916524986414713,-0.119330187030486,
0.534352034022757));
#17328=CARTESIAN_POINT('Ctrl Pts',(0.0505589280467443,-0.141716861518734,
0.542291023660064));
#17329=CARTESIAN_POINT('Ctrl Pts',(0.146487121137799,-0.0343714617774037,
0.550230013297369));
#17330=CARTESIAN_POINT('Ctrl Pts',(0.108316394245265,0.104438655591022,
0.558169002934674));
#17331=CARTESIAN_POINT('Ctrl Pts',(-0.0290105681715044,0.147642341414387,
0.566107992571982));
#17332=CARTESIAN_POINT('Ctrl Pts',(-0.139780343651344,0.0556895822633619,
0.574046982209285));
#17333=CARTESIAN_POINT('Ctrl Pts',(-0.122590794290966,-0.0872431727934394,
0.581985971846593));
#17334=CARTESIAN_POINT('Ctrl Pts',(0.00682222554696161,-0.150310782322966,
0.589924961483898));
#17335=CARTESIAN_POINT('Ctrl Pts',(0.129989965454297,-0.0757791721064987,
0.597863951121203));
#17336=CARTESIAN_POINT('Ctrl Pts',(0.134160800782372,0.0681230766876274,
0.60580294075851));
#17337=CARTESIAN_POINT('Ctrl Pts',(0.015516617634347,0.149663317553585,
0.613741930395814));
#17338=CARTESIAN_POINT('Ctrl Pts',(-0.117331965534667,0.0941970482962578,
0.621680920033121));
#17339=CARTESIAN_POINT('Ctrl Pts',(-0.142771175541451,-0.0475001629309618,
0.629619909670426));
#17340=CARTESIAN_POINT('Ctrl Pts',(-0.0375131590877193,-0.145714230393655,
0.637558899307733));
#17341=CARTESIAN_POINT('Ctrl Pts',(0.102085583566124,-0.110536906379362,
0.645497888945037));
#17342=CARTESIAN_POINT('Ctrl Pts',(0.148231970847143,0.0258293798362968,
0.653436878582344));
#17343=CARTESIAN_POINT('Ctrl Pts',(0.0586821478180281,0.138550639014834,
0.661375868219649));
#17344=CARTESIAN_POINT('Ctrl Pts',(-0.0845871597882484,0.124438283670714,
0.669314857856955));
#17345=CARTESIAN_POINT('Ctrl Pts',(-0.150422719745043,-0.00358879206139753,
0.67725384749426));
#17346=CARTESIAN_POINT('Ctrl Pts',(-0.078556588917505,-0.128330574617282,
0.685192837131567));
#17347=CARTESIAN_POINT('Ctrl Pts',(0.065222715229363,-0.135594511179713,
0.693131826768872));
#17348=CARTESIAN_POINT('Ctrl Pts',(0.149295093588351,-0.0187309656558678,
0.701070816406178));
#17349=CARTESIAN_POINT('Ctrl Pts',(0.0966980456281902,0.11527949520901,
0.709009806043483));
#17350=CARTESIAN_POINT('Ctrl Pts',(-0.044419435954706,0.14375947882982,
0.716948795680789));
#17351=CARTESIAN_POINT('Ctrl Pts',(-0.144873968183829,0.0406375120624596,
0.724887785318095));
#17352=CARTESIAN_POINT('Ctrl Pts',(-0.112706311402131,-0.099685311927494,
0.732826774955401));
#17353=CARTESIAN_POINT('Ctrl Pts',(0.0226362492002416,-0.148753064728429,
0.740765764592706));
#17354=CARTESIAN_POINT('Ctrl Pts',(0.137256875023267,-0.0616475814838108,
0.748704754230013));
#17355=CARTESIAN_POINT('Ctrl Pts',(0.126228238590478,0.0818920376245527,
0.756643743867318));
#17356=CARTESIAN_POINT('Ctrl Pts',(-0.000353699285724532,0.150465108715513,
0.764582733504624));
#17357=CARTESIAN_POINT('Ctrl Pts',(-0.126611849706441,0.0812976848247803,
0.772521723141928));
#17358=CARTESIAN_POINT('Ctrl Pts',(-0.136965528997667,-0.0622921978288208,
0.780460712779236));
#17359=CARTESIAN_POINT('Ctrl Pts',(-0.0219366533522686,-0.148857842533265,
0.788399702416541));
#17360=CARTESIAN_POINT('Ctrl Pts',(0.113173725020093,-0.0991543342927188,
0.796338692053846));
#17361=CARTESIAN_POINT('Ctrl Pts',(0.144681314438483,0.0413181715024817,
0.804277681691154));
#17362=CARTESIAN_POINT('Ctrl Pts',(0.0437430761464933,0.143966723006387,
0.812216671328456));
#17363=CARTESIAN_POINT('Ctrl Pts',(-0.0972389504488157,0.114823606281847,
0.820155660965765));
#17364=CARTESIAN_POINT('Ctrl Pts',(-0.149205382128735,-0.0194326526180533,
0.828094650603069));
#17365=CARTESIAN_POINT('Ctrl Pts',(-0.0645845121824554,-0.135899649852787,
0.836033640240376));
#17366=CARTESIAN_POINT('Ctrl Pts',(0.0791590524011713,-0.127959831458565,
0.843972629877681));
#17367=CARTESIAN_POINT('Ctrl Pts',(0.150437929635691,-0.00288155702400619,
0.851911619514986));
#17368=CARTESIAN_POINT('Ctrl Pts',(0.0840011924733913,0.12483458538003,
0.859850609152293));
#17369=CARTESIAN_POINT('Ctrl Pts',(-0.0593328794206009,0.138273220341526,
0.867789598789597));
#17370=CARTESIAN_POINT('Ctrl Pts',(-0.148351766552825,0.0251321985630355,
0.875728588426904));
#17371=CARTESIAN_POINT('Ctrl Pts',(-0.1015647786165,-0.111015628577859,
0.883667578064211));
#17372=CARTESIAN_POINT('Ctrl Pts',(0.0381978034543637,-0.145536256153639,
0.891606567701514));
#17373=CARTESIAN_POINT('Ctrl Pts',(0.142992914329196,-0.046828415471795,
0.899545557338823));
#17374=CARTESIAN_POINT('Ctrl Pts',(0.116887812080083,0.0947476302135675,
0.907484546976125));
#17375=CARTESIAN_POINT('Ctrl Pts',(-0.0162200712834111,0.149588713917584,
0.915423536613434));
#17376=CARTESIAN_POINT('Ctrl Pts',(-0.134479591021026,0.067491582014154,
0.923362526250738));
#17377=CARTESIAN_POINT('Ctrl Pts',(-0.129632261667175,-0.0763894677230377,
0.931301515888044));
#17378=CARTESIAN_POINT('Ctrl Pts',(-0.00611548103612966,-0.150341195071919,
0.93924050552535));
#17379=CARTESIAN_POINT('Ctrl Pts',(0.122999603362204,-0.0866658618874593,
0.947179495162656));
#17380=CARTESIAN_POINT('Ctrl Pts',(0.139516980595786,0.0563461282555487,
0.95511848479996));
#17381=CARTESIAN_POINT('Ctrl Pts',(0.0283161238170646,0.147777099632969,
0.963057474437267));
#17382=CARTESIAN_POINT('Ctrl Pts',(-0.108806203685475,0.103928264122473,
0.970996464074573));
#17383=CARTESIAN_POINT('Ctrl Pts',(-0.146323908690103,-0.0350597745230392,
0.978935453711877));
#17384=CARTESIAN_POINT('Ctrl Pts',(-0.049892103521326,-0.14195299239598,
0.986874443349185));
#17385=CARTESIAN_POINT('Ctrl Pts',(0.0922125030920605,-0.118897974404329,
0.994813432986488));
#17386=CARTESIAN_POINT('Ctrl Pts',(0.149902882860231,0.0129999905441286,
1.0027524226238));
#17387=CARTESIAN_POINT('Ctrl Pts',(0.0703674468853664,0.132997355096976,
1.0106914122611));
#17388=CARTESIAN_POINT('Ctrl Pts',(-0.0735845641169637,0.131244755962562,
1.01863040189841));
#17389=CARTESIAN_POINT('Ctrl Pts',(-0.150174949749745,0.00934657753497952,
1.02656939153571));
#17390=CARTESIAN_POINT('Ctrl Pts',(-0.0892904610481016,-0.121107752063083,
1.03450838117302));
#17391=CARTESIAN_POINT('Ctrl Pts',(0.0533333252681307,-0.140696234703703,
1.04244737081032));
#17392=CARTESIAN_POINT('Ctrl Pts',(0.147134107472884,-0.031486957015783,
1.05038636044763));
#17393=CARTESIAN_POINT('Ctrl Pts',(0.106243698045146,0.106546471877992,
1.05832535008494));
#17394=CARTESIAN_POINT('Ctrl Pts',(-0.0319055355867657,0.147043907874068,
1.06626433972224));
#17395=CARTESIAN_POINT('Ctrl Pts',(-0.14084743801815,0.0529327237885883,
1.07420332935955));
#17396=CARTESIAN_POINT('Ctrl Pts',(-0.120853163849259,-0.0896347412088629,
1.08214231899685));
#17397=CARTESIAN_POINT('Ctrl Pts',(0.00977389921538986,-0.150147743699608,
1.09008130863416));
#17398=CARTESIAN_POINT('Ctrl Pts',(0.13145362739741,-0.0732107771302755,
1.09802029827146));
#17399=CARTESIAN_POINT('Ctrl Pts',(0.132796568802552,0.0707456384395876,
1.10595928790877));
#17400=CARTESIAN_POINT('Ctrl Pts',(0.0125733526121963,0.149939270533256,
1.11389827754607));
#17401=CARTESIAN_POINT('Ctrl Pts',(-0.119159906186493,0.0918737764630459,
1.12183726718338));
#17402=CARTESIAN_POINT('Ctrl Pts',(-0.141810437433163,-0.0502958634379693,
1.12977625682069));
#17403=CARTESIAN_POINT('Ctrl Pts',(-0.0346432321137694,-0.146423087362162,
1.13771524645799));
#17404=CARTESIAN_POINT('Ctrl Pts',(0.104237477950025,-0.108510009835838,
1.1456542360953));
#17405=CARTESIAN_POINT('Ctrl Pts',(0.147695920811486,0.0287365450185451,
1.1535932257326));
#17406=CARTESIAN_POINT('Ctrl Pts',(0.0559488704325515,0.139676762352502,
1.16153221536991));
#17407=CARTESIAN_POINT('Ctrl Pts',(-0.0870155364008756,0.12275247642644,
1.16947120500722));
#17408=CARTESIAN_POINT('Ctrl Pts',(-0.150323183223479,-0.00654328889139735,
1.17741019464452));
#17409=CARTESIAN_POINT('Ctrl Pts',(-0.0760202581255566,-0.129849121670035,
1.18534918428183));
#17410=CARTESIAN_POINT('Ctrl Pts',(0.0678740032777675,-0.134286982701248,
1.19328817391913));
#17411=CARTESIAN_POINT('Ctrl Pts',(0.149634266389533,-0.0157943143574443,
1.20122716355644));
#17412=CARTESIAN_POINT('Ctrl Pts',(0.0944146137277022,0.117156966325547,
1.20916615319374));
#17413=CARTESIAN_POINT('Ctrl Pts',(-0.047235147145783,0.142859073628774,
1.21710514283105));
#17414=CARTESIAN_POINT('Ctrl Pts',(-0.145644368043342,0.037783489796601,
1.22504413246835));
#17415=CARTESIAN_POINT('Ctrl Pts',(-0.11072615165767,-0.101880289472715,
1.23298312210566));
#17416=CARTESIAN_POINT('Ctrl Pts',(0.0255542680118797,-0.148279646041953,
1.24092211174296));
#17417=CARTESIAN_POINT('Ctrl Pts',(0.138441506664824,-0.0589391489276913,
1.24886110138027));
#17418=CARTESIAN_POINT('Ctrl Pts',(0.124595033982396,0.0843560996663564,
1.25680009101758));
#17419=CARTESIAN_POINT('Ctrl Pts',(-0.00330965325590636,0.150429120316621,
1.26473908065488));
#17420=CARTESIAN_POINT('Ctrl Pts',(-0.128184579763139,0.0787945908985174,
1.27267807029219));
#17421=CARTESIAN_POINT('Ctrl Pts',(-0.135715308561414,-0.0649709863423027,
1.2806170599295));
#17422=CARTESIAN_POINT('Ctrl Pts',(-0.0190079735469551,-0.149260078337129,
1.2885560495668));
#17423=CARTESIAN_POINT('Ctrl Pts',(0.115099858543875,-0.0969117980795561,
1.29649503920411));
#17424=CARTESIAN_POINT('Ctrl Pts',(0.143841658454547,0.0441525915281748,
1.30443402884141));
#17425=CARTESIAN_POINT('Ctrl Pts',(0.0409062781470196,0.144798309552134,
1.31237301847872));
#17426=CARTESIAN_POINT('Ctrl Pts',(-0.0994759962839106,0.112891098884786,
1.32031200811602));
#17427=CARTESIAN_POINT('Ctrl Pts',(-0.148794813708878,-0.0223601759313527,
1.32825099775333));
#17428=CARTESIAN_POINT('Ctrl Pts',(-0.0619021766503053,-0.13714224202644,
1.33618998739064));
#17429=CARTESIAN_POINT('Ctrl Pts',(0.0816576604940555,-0.126379984705639,
1.34412897702794));
#17430=CARTESIAN_POINT('Ctrl Pts',(0.150465506209006,7.4487583413377E-5,
1.35206796666525));
#17431=CARTESIAN_POINT('Ctrl Pts',(0.0815324923277053,0.126460770918471,
1.36000695630255));
#17432=CARTESIAN_POINT('Ctrl Pts',(-0.062037929094705,0.137080886684378,
1.36794594593986));
#17433=CARTESIAN_POINT('Ctrl Pts',(-0.148816880822527,0.0222128430196456,
1.37588493557716));
#17434=CARTESIAN_POINT('Ctrl Pts',(-0.0993641722043223,-0.112989531455785,
1.38382392521447));
#17435=CARTESIAN_POINT('Ctrl Pts',(0.0410496166270677,-0.144757742348562,
1.39176291485178));
#17436=CARTESIAN_POINT('Ctrl Pts',(0.143885312916173,-0.0440101443352923,
1.39970190448908));
#17437=CARTESIAN_POINT('Ctrl Pts',(0.115003831846793,0.0970256929337524,
1.40764089412639));
#17438=CARTESIAN_POINT('Ctrl Pts',(-0.0191557100743377,0.149241218055048,
1.41557988376369));
#17439=CARTESIAN_POINT('Ctrl Pts',(-0.135779636557791,0.0648365220611291,
1.423518873401));
#17440=CARTESIAN_POINT('Ctrl Pts',(-0.128106375355825,-0.0789213496179777,
1.4314578630383));
#17441=CARTESIAN_POINT('Ctrl Pts',(-0.00316095527563228,-0.150432546011701,
1.43939685267561));
#17442=CARTESIAN_POINT('Ctrl Pts',(0.12467895337041,-0.0842322751882648,
1.44733584231291));
#17443=CARTESIAN_POINT('Ctrl Pts',(0.138382210043398,0.0590753877074232,
1.45527483195022));
#17444=CARTESIAN_POINT('Ctrl Pts',(0.0254091034322018,0.148306397458819,
1.46321382158753));
#17445=CARTESIAN_POINT('Ctrl Pts',(-0.110830116988615,0.101767718932792,
1.47115281122483));
#17446=CARTESIAN_POINT('Ctrl Pts',(-0.145600909330124,-0.0379221829034233,
1.47909180086214));
#17447=CARTESIAN_POINT('Ctrl Pts',(-0.0471050325108872,-0.142916194795756,
1.48703079049945));
#17448=CARTESIAN_POINT('Ctrl Pts',(0.0945521370959566,-0.117043625665234,
1.49496978013675));
#17449=CARTESIAN_POINT('Ctrl Pts',(0.14957741911039,0.0159047428854941,
1.50290876977406));
#17450=CARTESIAN_POINT('Ctrl Pts',(0.0678206238522695,0.134426714629862,
1.51084775941136));
#17451=CARTESIAN_POINT('Ctrl Pts',(-0.0763126473618499,0.129627546381738,
1.51878674904867));
#17452=CARTESIAN_POINT('Ctrl Pts',(-0.125385920115907,0.0477050348167321,
1.52407940880687));
#17453=CARTESIAN_POINT('Ctrl Pts',(-0.127184992207234,0.00540996832206346,
1.52672573868597));
#17454=CARTESIAN_POINT('Ctrl Pts',(0.0684664424539414,-0.095829519891843,
-1.38777878078145E-17));
#17455=CARTESIAN_POINT('Ctrl Pts',(0.100334321247169,-0.0730611673843044,
0.00264632987910189));
#17456=CARTESIAN_POINT('Ctrl Pts',(0.139021564822767,0.00636891437108143,
0.00793898963730573));
#17457=CARTESIAN_POINT('Ctrl Pts',(0.0699018669780613,0.120491966796142,
0.0158779792746114));
#17458=CARTESIAN_POINT('Ctrl Pts',(-0.0632645460347191,0.123954346655885,
0.0238169689119172));
#17459=CARTESIAN_POINT('Ctrl Pts',(-0.138486976988987,0.0141253725679007,
0.0317559585492228));
#17460=CARTESIAN_POINT('Ctrl Pts',(-0.0869496735326521,-0.108728403071097,
0.0396949481865287));
#17461=CARTESIAN_POINT('Ctrl Pts',(0.0441923146003338,-0.131999388615902,
0.0476339378238343));
#17462=CARTESIAN_POINT('Ctrl Pts',(0.134874939024977,-0.034459980695041,
0.0555729274611401));
#17463=CARTESIAN_POINT('Ctrl Pts',(0.102091080224759,0.094638871230671,
0.0635119170984456));
#17464=CARTESIAN_POINT('Ctrl Pts',(-0.0241513666277066,0.137095110112719,
0.0714509067357516));
#17465=CARTESIAN_POINT('Ctrl Pts',(-0.128284260007319,0.0540539703915629,
0.0793898963730571));
#17466=CARTESIAN_POINT('Ctrl Pts',(-0.114982038412656,-0.0784718756714057,
0.0873288860103631));
#17467=CARTESIAN_POINT('Ctrl Pts',(0.00357853460314598,-0.139161043603659,
0.0952678756476685));
#17468=CARTESIAN_POINT('Ctrl Pts',(0.118863112008681,-0.0724583686054966,
0.103206865284975));
#17469=CARTESIAN_POINT('Ctrl Pts',(0.125336705278751,0.0605752693714656,
0.11114585492228));
#17470=CARTESIAN_POINT('Ctrl Pts',(0.0170731091066207,0.138156245709763,
0.119084844559586));
#17471=CARTESIAN_POINT('Ctrl Pts',(-0.106819734848208,0.0892647286947484,
0.127023834196891));
#17472=CARTESIAN_POINT('Ctrl Pts',(-0.132926439498961,-0.0413425724611633,
0.134962823834197));
#17473=CARTESIAN_POINT('Ctrl Pts',(-0.0373480950846616,-0.134103559412242,
0.142901813471503));
#17474=CARTESIAN_POINT('Ctrl Pts',(0.0924198687735613,-0.104101940294199,
0.150840803108809));
#17475=CARTESIAN_POINT('Ctrl Pts',(0.137583777756591,0.0211978768359354,
0.158779792746114));
#17476=CARTESIAN_POINT('Ctrl Pts',(0.0567991668878991,0.127092487218924,
0.16671878238342));
#17477=CARTESIAN_POINT('Ctrl Pts',(-0.075981188277068,0.116642637502503,
0.174657772020726));
#17478=CARTESIAN_POINT('Ctrl Pts',(-0.139205973057234,-0.000585553717998882,
0.182596761658032));
#17479=CARTESIAN_POINT('Ctrl Pts',(-0.0749972298318695,-0.11727771015962,
0.190535751295337));
#17480=CARTESIAN_POINT('Ctrl Pts',(0.0578663373665801,-0.126610160769685,
0.198474740932643));
#17481=CARTESIAN_POINT('Ctrl Pts',(0.13775723856723,-0.0200396862227523,
0.206413730569949));
#17482=CARTESIAN_POINT('Ctrl Pts',(0.091540828968026,0.104875747581476,
0.214352720207254));
#17483=CARTESIAN_POINT('Ctrl Pts',(-0.0384749358425138,0.133784622116252,
0.22229170984456));
#17484=CARTESIAN_POINT('Ctrl Pts',(-0.133269533752038,0.0402228439430644,
0.230230699481866));
#17485=CARTESIAN_POINT('Ctrl Pts',(-0.106065007067505,-0.0901601911982067,
0.238169689119172));
#17486=CARTESIAN_POINT('Ctrl Pts',(0.0182347644767634,-0.138007750384372,
0.246108678756477));
#17487=CARTESIAN_POINT('Ctrl Pts',(0.125841858853055,-0.0595186723796334,
0.254047668393783));
#17488=CARTESIAN_POINT('Ctrl Pts',(0.118249355954961,0.073455671106145,
0.261986658031089));
#17489=CARTESIAN_POINT('Ctrl Pts',(0.00240767183786234,0.139186381940956,
0.269925647668394));
#17490=CARTESIAN_POINT('Ctrl Pts',(-0.115638070838342,0.0775014991741366,
0.277864637305701));
#17491=CARTESIAN_POINT('Ctrl Pts',(-0.12782508485658,-0.0551306945617612,
0.285803626943006));
#17492=CARTESIAN_POINT('Ctrl Pts',(-0.0229969941138309,-0.137294515779738,
0.293742616580312));
#17493=CARTESIAN_POINT('Ctrl Pts',(0.102883268653204,-0.0937746172089793,
0.301681606217617));
#17494=CARTESIAN_POINT('Ctrl Pts',(0.134580950019115,0.0355895166223291,
0.309620595854923));
#17495=CARTESIAN_POINT('Ctrl Pts',(0.0430789950773988,0.13237388709478,
0.317559585492229));
#17496=CARTESIAN_POINT('Ctrl Pts',(-0.0878588274613298,0.107979036106918,
0.325498575129534));
#17497=CARTESIAN_POINT('Ctrl Pts',(-0.1383679148179,-0.0152632221501787,
0.33343756476684));
#17498=CARTESIAN_POINT('Ctrl Pts',(-0.0622106591311991,-0.12453304658572,
0.341376554404146));
#17499=CARTESIAN_POINT('Ctrl Pts',(0.0708961914151981,-0.119801401679107,
0.349315544041452));
#17500=CARTESIAN_POINT('Ctrl Pts',(0.1391024375543,-0.00539978406154301,
0.357254533678757));
#17501=CARTESIAN_POINT('Ctrl Pts',(0.0799699354250877,0.113944965792994,
0.365193523316063));
#17502=CARTESIAN_POINT('Ctrl Pts',(-0.0523695618881846,0.128980908622551,
0.373132512953369));
#17503=CARTESIAN_POINT('Ctrl Pts',(-0.136768314413298,0.0259436692471295,
0.381071502590675));
#17504=CARTESIAN_POINT('Ctrl Pts',(-0.0959650484377783,-0.100843221288265,
0.38901049222798));
#17505=CARTESIAN_POINT('Ctrl Pts',(0.0326876424682324,-0.135315053971568,
0.396949481865287));
#17506=CARTESIAN_POINT('Ctrl Pts',(0.13141703692502,-0.0459152284901983,
0.404888471502591));
#17507=CARTESIAN_POINT('Ctrl Pts',(0.109843140674695,0.0855168418978295,
0.412827461139898));
#17508=CARTESIAN_POINT('Ctrl Pts',(-0.0122846228212416,0.13866410438033,
0.420766450777203));
#17509=CARTESIAN_POINT('Ctrl Pts',(-0.123166656044517,0.0648738825743514,
0.428705440414509));
#17510=CARTESIAN_POINT('Ctrl Pts',(-0.121298056821252,-0.0683039326309071,
0.436644430051815));
#17511=CARTESIAN_POINT('Ctrl Pts',(-0.00838939967687663,-0.138954178686792,
0.44458341968912));
#17512=CARTESIAN_POINT('Ctrl Pts',(0.11219917790857,-0.0824013973067221,
0.452522409326426));
#17513=CARTESIAN_POINT('Ctrl Pts',(0.13007709763057,0.0495842159710775,
0.460461398963732));
#17514=CARTESIAN_POINT('Ctrl Pts',(0.0288783492374893,0.136178877755608,
0.468400388601037));
#17515=CARTESIAN_POINT('Ctrl Pts',(-0.0987565487199846,0.0981111099028881,
0.476339378238344));
#17516=CARTESIAN_POINT('Ctrl Pts',(-0.135986594552616,-0.0297706550724338,
0.484278367875649));
#17517=CARTESIAN_POINT('Ctrl Pts',(-0.0487302328423073,-0.130399425645183,
0.492217357512954));
#17518=CARTESIAN_POINT('Ctrl Pts',(0.0831353173341669,-0.111656458896056,
0.50015634715026));
#17519=CARTESIAN_POINT('Ctrl Pts',(0.13889618212661,0.00930034365552528,
0.508095336787567));
#17520=CARTESIAN_POINT('Ctrl Pts',(0.0675071113591811,0.12174331898465,
0.516034326424871));
#17521=CARTESIAN_POINT('Ctrl Pts',(-0.0656800932930844,0.122738629397884,
0.523973316062178));
#17522=CARTESIAN_POINT('Ctrl Pts',(-0.138741673886299,0.0113751364249866,
0.531912305699483));
#17523=CARTESIAN_POINT('Ctrl Pts',(-0.0847947606245053,-0.110401514355972,
0.539851295336789));
#17524=CARTESIAN_POINT('Ctrl Pts',(0.0467759446245483,-0.131113145053959,
0.547790284974095));
#17525=CARTESIAN_POINT('Ctrl Pts',(0.135526478334676,-0.031799677225719,
0.555729274611401));
#17526=CARTESIAN_POINT('Ctrl Pts',(0.100211809365564,0.0966242157284558,
0.563668264248707));
#17527=CARTESIAN_POINT('Ctrl Pts',(-0.0268399031138932,0.136595261273209,
0.571607253886012));
#17528=CARTESIAN_POINT('Ctrl Pts',(-0.129321523751272,0.0515227066069736,
0.579546243523318));
#17529=CARTESIAN_POINT('Ctrl Pts',(-0.113418152377209,-0.0807153548762533,
0.587485233160623));
#17530=CARTESIAN_POINT('Ctrl Pts',(0.00631176444456456,-0.139064040754811,
0.595424222797929));
#17531=CARTESIAN_POINT('Ctrl Pts',(0.120263693490807,-0.0701091280034811,
0.603363212435234));
#17532=CARTESIAN_POINT('Ctrl Pts',(0.124122453355413,0.0630258865426945,
0.611302202072541));
#17533=CARTESIAN_POINT('Ctrl Pts',(0.0143556138404206,0.138465021405133,
0.619241191709845));
#17534=CARTESIAN_POINT('Ctrl Pts',(-0.108552806291007,0.0871489187988374,
0.627180181347153));
#17535=CARTESIAN_POINT('Ctrl Pts',(-0.132088571872698,-0.043946046262323,
0.635119170984457));
#17536=CARTESIAN_POINT('Ctrl Pts',(-0.0347063025259737,-0.134811417789573,
0.643058160621763));
#17537=CARTESIAN_POINT('Ctrl Pts',(0.0944472082050275,-0.102266175560326,
0.65099715025907));
#17538=CARTESIAN_POINT('Ctrl Pts',(0.137140772714236,0.0238967416356601,
0.658936139896373));
#17539=CARTESIAN_POINT('Ctrl Pts',(0.054291358674537,0.128183829614862,
0.666875129533682));
#17540=CARTESIAN_POINT('Ctrl Pts',(-0.0782580734018908,0.115127406593233,
0.674814119170985));
#17541=CARTESIAN_POINT('Ctrl Pts',(-0.139167602654929,-0.00332026696803425,
0.682753108808293));
#17542=CARTESIAN_POINT('Ctrl Pts',(-0.0726787294560835,-0.118728463672822,
0.690692098445597));
#17543=CARTESIAN_POINT('Ctrl Pts',(0.0603425395611779,-0.125448888878168,
0.698631088082904));
#17544=CARTESIAN_POINT('Ctrl Pts',(0.138124349154501,-0.0173294538893964,
0.706570077720209));
#17545=CARTESIAN_POINT('Ctrl Pts',(0.0894627833767505,0.106653908470079,
0.714509067357515));
#17546=CARTESIAN_POINT('Ctrl Pts',(-0.0410958292974484,0.133002927094911,
0.72244805699482));
#17547=CARTESIAN_POINT('Ctrl Pts',(-0.134034026730954,0.0375968812502473,
0.730387046632127));
#17548=CARTESIAN_POINT('Ctrl Pts',(-0.104273258644039,-0.0922265326964679,
0.738326036269432));
#17549=CARTESIAN_POINT('Ctrl Pts',(0.0209425314183671,-0.137622876656644,
0.746265025906738));
#17550=CARTESIAN_POINT('Ctrl Pts',(0.126986869252672,-0.0570349089493802,
0.754204015544043));
#17551=CARTESIAN_POINT('Ctrl Pts',(0.11678343126468,0.0757646090434518,
0.762143005181349));
#17552=CARTESIAN_POINT('Ctrl Pts',(-0.000327234354877375,0.139206819944772,
0.770081994818654));
#17553=CARTESIAN_POINT('Ctrl Pts',(-0.117138339349379,0.0752147276530931,
0.778020984455961));
#17554=CARTESIAN_POINT('Ctrl Pts',(-0.126717322684213,-0.0576312930030564,
0.785959974093266));
#17555=CARTESIAN_POINT('Ctrl Pts',(-0.0202952816069424,-0.137719814645367,
0.793898963730571));
#17556=CARTESIAN_POINT('Ctrl Pts',(0.104705698854998,-0.0917352845351548,
0.801837953367879));
#17557=CARTESIAN_POINT('Ctrl Pts',(0.133855787965376,0.0382266115373486,
0.809776943005182));
#17558=CARTESIAN_POINT('Ctrl Pts',(0.0404700769297216,0.133194664588195,
0.81771593264249));
#17559=CARTESIAN_POINT('Ctrl Pts',(-0.0899632159395838,0.106232130635072,
0.825654922279794));
#17560=CARTESIAN_POINT('Ctrl Pts',(-0.13804135019805,-0.0179786383510676,
0.833593911917101));
#17561=CARTESIAN_POINT('Ctrl Pts',(-0.059752088941783,-0.125731196083361,
0.841532901554406));
#17562=CARTESIAN_POINT('Ctrl Pts',(0.0732361146625898,-0.118385460722959,
0.849471891191712));
#17563=CARTESIAN_POINT('Ctrl Pts',(0.139181674492094,-0.00266594955618734,
0.857410880829018));
#17564=CARTESIAN_POINT('Ctrl Pts',(0.077715950067195,0.115494055719818,
0.865349870466323));
#17565=CARTESIAN_POINT('Ctrl Pts',(-0.0548934004223171,0.127927168308903,
0.87328886010363));
#17566=CARTESIAN_POINT('Ctrl Pts',(-0.137251604915624,0.0232517257326144,
0.881227849740934));
#17567=CARTESIAN_POINT('Ctrl Pts',(-0.0939653715754795,-0.102709078207047,
0.889166839378241));
#17568=CARTESIAN_POINT('Ctrl Pts',(0.0353397195745277,-0.134646760160997,
0.897105829015547));
#17569=CARTESIAN_POINT('Ctrl Pts',(0.132293719443212,-0.0433245611326863,
0.905044818652852));
#17570=CARTESIAN_POINT('Ctrl Pts',(0.108141885842356,0.0876583043865096,
0.912983808290157));
#17571=CARTESIAN_POINT('Ctrl Pts',(-0.0150064327997127,0.138395999855801,
0.920922797927463));
#17572=CARTESIAN_POINT('Ctrl Pts',(-0.124417390671652,0.0624416423544169,
0.928861787564769));
#17573=CARTESIAN_POINT('Ctrl Pts',(-0.119932754264349,-0.0706737593172073,
0.936800777202075));
#17574=CARTESIAN_POINT('Ctrl Pts',(-0.00565790085648466,-0.139092177922979,
0.944739766839381));
#17575=CARTESIAN_POINT('Ctrl Pts',(0.113796373024222,-0.0801812402497705,
0.952678756476687));
#17576=CARTESIAN_POINT('Ctrl Pts',(0.129077866376032,0.0521301276928276,
0.960617746113992));
#17577=CARTESIAN_POINT('Ctrl Pts',(0.026197419344502,0.13671993644362,0.968556735751298));
#17578=CARTESIAN_POINT('Ctrl Pts',(-0.100664969670515,0.0961520134094621,
0.976495725388603));
#17579=CARTESIAN_POINT('Ctrl Pts',(-0.13537547797311,-0.0324364881732178,
0.98443471502591));
#17580=CARTESIAN_POINT('Ctrl Pts',(-0.0461590140787468,-0.131331607851033,
0.992373704663214));
#17581=CARTESIAN_POINT('Ctrl Pts',(0.0853128637208732,-0.110001641284132,
1.00031269430052));
#17582=CARTESIAN_POINT('Ctrl Pts',(0.138686661656432,0.0120272889735618,
1.00825168393783));
#17583=CARTESIAN_POINT('Ctrl Pts',(0.0651023256631918,0.123046060459907,
1.01619067357513));
#17584=CARTESIAN_POINT('Ctrl Pts',(-0.0680787277209358,0.121424596492465,
1.02412966321244));
#17585=CARTESIAN_POINT('Ctrl Pts',(-0.138938371616466,0.00864723620724691,
1.03206865284975));
#17586=CARTESIAN_POINT('Ctrl Pts',(-0.0826094583655966,-0.112046076191904,
1.04000764248705));
#17587=CARTESIAN_POINT('Ctrl Pts',(0.0493427524230464,-0.130168884856471,
1.04794663212436));
#17588=CARTESIAN_POINT('Ctrl Pts',(0.136125055048066,-0.0291310004912345,
1.05588562176166));
#17589=CARTESIAN_POINT('Ctrl Pts',(0.0982941990358779,0.0985743183458784,
1.06382461139897));
#17590=CARTESIAN_POINT('Ctrl Pts',(-0.0295182596522469,0.136041604476578,
1.07176360103627));
#17591=CARTESIAN_POINT('Ctrl Pts',(-0.130308774647192,0.0489721252490281,
1.07970259067358));
#17592=CARTESIAN_POINT('Ctrl Pts',(-0.111810537096203,-0.0829279783650712,
1.08764158031088));
#17593=CARTESIAN_POINT('Ctrl Pts',(0.00904258428980543,-0.13891320121148,
1.09558056994819));
#17594=CARTESIAN_POINT('Ctrl Pts',(0.121617839487272,-0.067732908692211,
1.1035195595855));
#17595=CARTESIAN_POINT('Ctrl Pts',(0.122860297649024,0.0654522196953821,
1.1114585492228));
#17596=CARTESIAN_POINT('Ctrl Pts',(0.0116325734791967,0.138720326685422,
1.11939753886011));
#17597=CARTESIAN_POINT('Ctrl Pts',(-0.110243974478508,0.0849994817198388,
1.12733652849741));
#17598=CARTESIAN_POINT('Ctrl Pts',(-0.131199719314147,-0.0465325633653302,
1.13527551813472));
#17599=CARTESIAN_POINT('Ctrl Pts',(-0.0320511128216771,-0.13546723577438,
1.14321450777202));
#17600=CARTESIAN_POINT('Ctrl Pts',(0.0964380908528195,-0.100390938007982,
1.15115349740933));
#17601=CARTESIAN_POINT('Ctrl Pts',(0.136644831685568,0.0265863832644056,
1.15909248704664));
#17602=CARTESIAN_POINT('Ctrl Pts',(0.0517625939920979,0.129225692742072,
1.16703147668394));
#17603=CARTESIAN_POINT('Ctrl Pts',(-0.0805047509788913,0.113567736929491,
1.17497046632125));
#17604=CARTESIAN_POINT('Ctrl Pts',(-0.139075513779617,-0.00605369873671642,
1.18290945595855));
#17605=CARTESIAN_POINT('Ctrl Pts',(-0.0703321751825429,-0.12013338809653,
1.19084844559586));
#17606=CARTESIAN_POINT('Ctrl Pts',(0.0627954496153871,-0.124239193932754,
1.19878743523316));
#17607=CARTESIAN_POINT('Ctrl Pts',(0.138438143943654,-0.0146125323915816,
1.20672642487047));
#17608=CARTESIAN_POINT('Ctrl Pts',(0.0873502052771435,0.108390901091839,
1.21466541450777));
#17609=CARTESIAN_POINT('Ctrl Pts',(-0.043700859820065,0.132169893139269,
1.22260440414508));
#17610=CARTESIAN_POINT('Ctrl Pts',(-0.134746782767514,0.0349564062120582,
1.23054339378239));
#17611=CARTESIAN_POINT('Ctrl Pts',(-0.102441260891455,-0.0942572748833364,
1.23848238341969));
#17612=CARTESIAN_POINT('Ctrl Pts',(0.0236422145726536,-0.137184880695923,
1.246421373057));
#17613=CARTESIAN_POINT('Ctrl Pts',(0.128082862902196,-0.0545291301253663,
1.2543603626943));
#17614=CARTESIAN_POINT('Ctrl Pts',(0.115272428336817,0.0780443019497631,
1.26229935233161));
#17615=CARTESIAN_POINT('Ctrl Pts',(-0.00306201423577413,0.139173524314926,
1.27023834196891));
#17616=CARTESIAN_POINT('Ctrl Pts',(-0.118593392628464,0.0728989233548558,
1.27817733160622));
#17617=CARTESIAN_POINT('Ctrl Pts',(-0.125560647806918,-0.06010964584811,
1.28611632124353));
#17618=CARTESIAN_POINT('Ctrl Pts',(-0.0175857351491984,-0.138091953858251,
1.29405531088083));
#17619=CARTESIAN_POINT('Ctrl Pts',(0.106487712804436,-0.089660542174548,
1.30199430051814));
#17620=CARTESIAN_POINT('Ctrl Pts',(0.133078957772855,0.0408489510387311,
1.30993329015544));
#17621=CARTESIAN_POINT('Ctrl Pts',(0.0378455373822902,0.133964029124136,
1.31787227979275));
#17622=CARTESIAN_POINT('Ctrl Pts',(-0.0920328787300654,0.104444219726284,
1.32581126943006));
#17623=CARTESIAN_POINT('Ctrl Pts',(-0.137661501842601,-0.0206871148492911,
1.33375025906736));
#17624=CARTESIAN_POINT('Ctrl Pts',(-0.0572704544775333,-0.126880813469472,
1.34168924870467));
#17625=CARTESIAN_POINT('Ctrl Pts',(0.0755477687720905,-0.116923823242002,
1.34962823834197));
#17626=CARTESIAN_POINT('Ctrl Pts',(0.13920718769651,6.89141801743488E-5,
1.35756722797928));
#17627=CARTESIAN_POINT('Ctrl Pts',(0.0754319660950179,0.116998564767658,
1.36550621761658));
#17628=CARTESIAN_POINT('Ctrl Pts',(-0.0573960494825499,0.126824048933643,
1.37344520725389));
#17629=CARTESIAN_POINT('Ctrl Pts',(-0.13768191782304,0.0205508058651932,
1.38138419689119));
#17630=CARTESIAN_POINT('Ctrl Pts',(-0.0919294216917856,-0.104535287252199,
1.3893231865285));
#17631=CARTESIAN_POINT('Ctrl Pts',(0.0379781508110965,-0.133926497290667,
1.39726217616581));
#17632=CARTESIAN_POINT('Ctrl Pts',(0.133119345865688,-0.0407171622080862,
1.40520116580311));
#17633=CARTESIAN_POINT('Ctrl Pts',(0.106398871137127,0.0897659150453452,
1.41314015544042));
#17634=CARTESIAN_POINT('Ctrl Pts',(-0.0177224175491345,0.138074504763813,
1.42107914507772));
#17635=CARTESIAN_POINT('Ctrl Pts',(-0.125620162573399,0.0599852426217579,
1.42901813471503));
#17636=CARTESIAN_POINT('Ctrl Pts',(-0.118521039729242,-0.0730161975746823,
1.43695712435233));
#17637=CARTESIAN_POINT('Ctrl Pts',(-0.00292444232197888,-0.139176693688359,
1.44489611398964));
#17638=CARTESIAN_POINT('Ctrl Pts',(0.115350068603298,-0.0779297424218237,
1.45283510362695));
#17639=CARTESIAN_POINT('Ctrl Pts',(0.128028003046829,0.0546551750765237,
1.46077409326425));
#17640=CARTESIAN_POINT('Ctrl Pts',(0.0235079116789307,0.137209630484779,
1.46871308290156));
#17641=CARTESIAN_POINT('Ctrl Pts',(-0.102537447198224,0.0941531272373115,
1.47665207253886));
#17642=CARTESIAN_POINT('Ctrl Pts',(-0.134706575776555,-0.0350847218495708,
1.48459106217617));
#17643=CARTESIAN_POINT('Ctrl Pts',(-0.0435804807853106,-0.132222740314769,
1.49253005181348));
#17644=CARTESIAN_POINT('Ctrl Pts',(0.0874774386997331,-0.108286040948335,
1.50046904145078));
#17645=CARTESIAN_POINT('Ctrl Pts',(0.138385550162814,0.0147146982980264,
1.50840803108809));
#17646=CARTESIAN_POINT('Ctrl Pts',(0.0627460642121078,0.124368470664037,
1.51634702072539));
#17647=CARTESIAN_POINT('Ctrl Pts',(-0.0706026869052757,0.119928391791904,
1.5242860103627));
#17648=CARTESIAN_POINT('Ctrl Pts',(-0.116004137797729,0.0441355889673283,
1.5295786701209));
#17649=CARTESIAN_POINT('Ctrl Pts',(-0.117668597464313,0.00500517689812487,
1.532225));
#17650=CARTESIAN_POINT('',(0.0684664424539461,-0.0958295198918396,0.));
#17651=CARTESIAN_POINT('Ctrl Pts',(0.0684664424539414,-0.095829519891843,
-1.38777878078145E-17));
#17652=CARTESIAN_POINT('Ctrl Pts',(0.100334321247169,-0.0730611673843044,
0.00264632987910189));
#17653=CARTESIAN_POINT('Ctrl Pts',(0.139021564822767,0.00636891437108143,
0.00793898963730573));
#17654=CARTESIAN_POINT('Ctrl Pts',(0.0699018669780613,0.120491966796142,
0.0158779792746114));
#17655=CARTESIAN_POINT('Ctrl Pts',(-0.0632645460347191,0.123954346655885,
0.0238169689119172));
#17656=CARTESIAN_POINT('Ctrl Pts',(-0.11596266760442,0.0470121293552651,
0.0293787386625077));
#17657=CARTESIAN_POINT('Ctrl Pts',(-0.117944740497024,0.00404481602818191,
0.0322941785339964));
#17658=CARTESIAN_POINT('Ctrl Pts',(-0.117917485785546,7.60014832213644E-5,
0.0325632885263832));
#17659=CARTESIAN_POINT('Ctrl Pts',(0.0635546915223951,0.132092229195826,
-2.16840434497101E-19));
#17660=CARTESIAN_POINT('Ctrl Pts',(0.0668114782730532,0.13015255741457,
-1.00603861447787E-18));
#17661=CARTESIAN_POINT('Ctrl Pts',(0.0699821360194518,0.12808121947321,
-2.9262196004085E-17));
#17662=CARTESIAN_POINT('Ctrl Pts',(0.0730575207853233,0.125877721325919,
-2.71050543121376E-17));
#17663=CARTESIAN_POINT('Ctrl Pts',(0.0789281193465506,0.121671466161783,
-2.36378102375718E-17));
#17664=CARTESIAN_POINT('Ctrl Pts',(0.0844522091809674,0.11698398814956,
1.43782932504085E-18));
#17665=CARTESIAN_POINT('Ctrl Pts',(0.0895990070394484,0.111875963994554,
9.97465998686664E-18));
#17666=CARTESIAN_POINT('Ctrl Pts',(0.0928865546640729,0.108613183302742,
1.54276111490851E-17));
#17667=CARTESIAN_POINT('Ctrl Pts',(0.0960206821069302,0.105176950779614,
-2.53636710091701E-17));
#17668=CARTESIAN_POINT('Ctrl Pts',(0.098978417360439,0.101599719103904,
-1.56125112837913E-17));
#17669=CARTESIAN_POINT('Ctrl Pts',(0.103148772110026,0.0965558852815647,
-1.86354736740503E-18));
#17670=CARTESIAN_POINT('Ctrl Pts',(0.106976174326278,0.0912251680483688,
1.1337629845105E-17));
#17671=CARTESIAN_POINT('Ctrl Pts',(0.110435561611279,0.0856523061447448,
2.03830008427275E-17));
#17672=CARTESIAN_POINT('Ctrl Pts',(0.112407683932559,0.0824753373788608,
2.55395723911076E-17));
#17673=CARTESIAN_POINT('Ctrl Pts',(0.114261188142284,0.0792174064057451,
2.29308760465575E-17));
#17674=CARTESIAN_POINT('Ctrl Pts',(0.115986535786665,0.0758936579718971,
2.08166817117217E-17));
#17675=CARTESIAN_POINT('Ctrl Pts',(0.120573220307724,0.0670577659456877,
1.51962825639422E-17));
#17676=CARTESIAN_POINT('Ctrl Pts',(0.124235263225439,0.0578042025119142,
2.52358375750583E-18));
#17677=CARTESIAN_POINT('Ctrl Pts',(0.126883306113679,0.0482911783993335,
1.30104260698261E-17));
#17678=CARTESIAN_POINT('Ctrl Pts',(0.128478610866444,0.0425600882242624,
1.93281898253259E-17));
#17679=CARTESIAN_POINT('Ctrl Pts',(0.129704960854084,0.0367345196138549,
-5.78096029915021E-19));
#17680=CARTESIAN_POINT('Ctrl Pts',(0.130533291754837,0.0308494671050701,
0.));
#17681=CARTESIAN_POINT('Ctrl Pts',(0.131003715791213,0.0275072397983871,
3.2831114661813E-19));
#17682=CARTESIAN_POINT('Ctrl Pts',(0.131345346899704,0.0241444941465381,
-1.7128612844445E-18));
#17683=CARTESIAN_POINT('Ctrl Pts',(0.131551728167405,0.0207857616715298,
2.60208521396521E-18));
#17684=CARTESIAN_POINT('Ctrl Pts',(0.131851321606701,0.0159100565018035,
8.86587880453295E-18));
#17685=CARTESIAN_POINT('Ctrl Pts',(0.131867617692795,0.0110341713389591,
-1.68111772803455E-17));
#17686=CARTESIAN_POINT('Ctrl Pts',(0.131586936334964,0.0061777758930637,
-6.93889390390723E-18));
#17687=CARTESIAN_POINT('Ctrl Pts',(0.131099036368572,-0.00226395031615145,
9.98510028643051E-18));
#17688=CARTESIAN_POINT('Ctrl Pts',(0.129715139118287,-0.0106479390144509,
1.03491660509995E-17));
#17689=CARTESIAN_POINT('Ctrl Pts',(0.127493709984164,-0.018859987399606,
1.04083408558608E-17));
#17690=CARTESIAN_POINT('Ctrl Pts',(0.126553994220251,-0.0223338732882013,
1.04333731632617E-17));
#17691=CARTESIAN_POINT('Ctrl Pts',(0.125463061762623,-0.0257782540966497,
1.75224609115742E-17));
#17692=CARTESIAN_POINT('Ctrl Pts',(0.124232565886791,-0.0291638780753137,
1.73472347597681E-17));
#17693=CARTESIAN_POINT('Ctrl Pts',(0.12170396813588,-0.0361211392462112,
1.69871551674183E-17));
#17694=CARTESIAN_POINT('Ctrl Pts',(0.118582485980247,-0.0428512226170345,
-6.45748389186585E-19));
#17695=CARTESIAN_POINT('Ctrl Pts',(0.114911168983798,-0.0492778939609075,
3.46944695195361E-18));
#17696=CARTESIAN_POINT('Ctrl Pts',(0.112347970921096,-0.0537647937721124,
6.34254691478841E-18));
#17697=CARTESIAN_POINT('Ctrl Pts',(0.109516356061708,-0.0581036184196785,
-1.05628593522785E-17));
#17698=CARTESIAN_POINT('Ctrl Pts',(0.106427098863261,-0.0622637901458048,
-1.21430643318376E-17));
#17699=CARTESIAN_POINT('Ctrl Pts',(0.104287070791936,-0.0651456752410043,
-1.32377232732828E-17));
#17700=CARTESIAN_POINT('Ctrl Pts',(0.102021590876101,-0.067943056099314,
-1.03088264066386E-17));
#17701=CARTESIAN_POINT('Ctrl Pts',(0.0996491962474235,-0.0706287444932102,
-1.04083408558608E-17));
#17702=CARTESIAN_POINT('Ctrl Pts',(0.0938611946766418,-0.0771810981592459,
-1.06511292104842E-17));
#17703=CARTESIAN_POINT('Ctrl Pts',(0.0874218747326319,-0.0830961188460978,
9.460259835177E-18));
#17704=CARTESIAN_POINT('Ctrl Pts',(0.0803902102994179,-0.0882260767030795,
2.94902990916057E-17));
#17705=CARTESIAN_POINT('Ctrl Pts',(0.0765868618375105,-0.091000813397402,
4.03243227742548E-17));
#17706=CARTESIAN_POINT('Ctrl Pts',(0.0726097989303321,-0.0935451549285004,
-2.49510848448888E-18));
#17707=CARTESIAN_POINT('Ctrl Pts',(0.0684664424539416,-0.0958295198918429,
0.));
#17708=CARTESIAN_POINT('Ctrl Pts',(-0.00156962371674571,0.146072546381438,
1.50365));
#17709=CARTESIAN_POINT('Ctrl Pts',(0.0218361081466035,0.146362061217761,
1.50238307892777));
#17710=CARTESIAN_POINT('Ctrl Pts',(0.0452966847593804,0.141345883428421,
1.50111615785553));
#17711=CARTESIAN_POINT('Ctrl Pts',(0.0660179268768178,0.130913916311315,
1.4998492367833));
#17712=CARTESIAN_POINT('Ctrl Pts',(0.109300214423576,0.109123745727819,
1.4972029069042));
#17713=CARTESIAN_POINT('Ctrl Pts',(0.140630685714559,0.0637042888941242,
1.49455657702509));
#17714=CARTESIAN_POINT('Ctrl Pts',(0.145752650840527,0.0155206226173656,
1.49191024714599));
#17715=CARTESIAN_POINT('Ctrl Pts',(0.150874615966495,-0.0326630436593903,
1.48926391726689));
#17716=CARTESIAN_POINT('Ctrl Pts',(0.129788074927449,-0.0836109193792113,
1.48661758738779));
#17717=CARTESIAN_POINT('Ctrl Pts',(0.0921021927661857,-0.114042242015571,
1.48397125750869));
#17718=CARTESIAN_POINT('Ctrl Pts',(0.0544163106049216,-0.144473564651931,
1.48132492762959));
#17719=CARTESIAN_POINT('Ctrl Pts',(0.000131087321441313,-0.154388334204831,
1.47867859775048));
#17720=CARTESIAN_POINT('Ctrl Pts',(-0.0458840977328367,-0.139228052523514,
1.47603226787138));
#17721=CARTESIAN_POINT('Ctrl Pts',(-0.0918992827871148,-0.124067770842196,
1.47338593799228));
#17722=CARTESIAN_POINT('Ctrl Pts',(-0.129644429612189,-0.0838324379266627,
1.47073960811318));
#17723=CARTESIAN_POINT('Ctrl Pts',(-0.141854649713415,-0.0369491035797489,
1.46809327823408));
#17724=CARTESIAN_POINT('Ctrl Pts',(-0.14497337938942,-0.0249741805295802,
1.46741735368415));
#17725=CARTESIAN_POINT('Ctrl Pts',(-0.146426231435716,-0.0125655473306973,
1.46674142913422));
#17726=CARTESIAN_POINT('Ctrl Pts',(-0.14631473222987,-0.000131398079681141,
1.46606550458429));
#17727=CARTESIAN_POINT('Origin',(0.,0.,-0.0924367114736175));
#17728=CARTESIAN_POINT('',(-0.0684664424539507,-0.0958295198918364,0.));
#17729=CARTESIAN_POINT('Ctrl Pts',(-0.0686146973663072,-0.0959584553529141,
8.16675286424706E-17));
#17730=CARTESIAN_POINT('Ctrl Pts',(-0.0391968190522335,-0.116741470120209,
0.00244290680874874));
#17731=CARTESIAN_POINT('Ctrl Pts',(0.0436301113039178,-0.130476273073809,
0.0075332029917574));
#17732=CARTESIAN_POINT('Ctrl Pts',(0.134092250525203,-0.0374520209666004,
0.0152708885490261));
#17733=CARTESIAN_POINT('Ctrl Pts',(0.104134301645602,0.0924305194826295,
0.023213056671806));
#17734=CARTESIAN_POINT('Ctrl Pts',(-0.0212379681243542,0.137589894578696,
0.0311552247945861));
#17735=CARTESIAN_POINT('Ctrl Pts',(-0.106685947947232,0.0723488109778776,
0.0375631097285225));
#17736=CARTESIAN_POINT('Ctrl Pts',(-0.117663533972591,0.0165813593984342,
0.041323605288199));
#17737=CARTESIAN_POINT('Ctrl Pts',(-0.117600989619072,5.04992496179954E-5,
0.0424367114736154));
#17738=CARTESIAN_POINT('Origin',(0.,0.,0.));
#17739=CARTESIAN_POINT('Ctrl Pts',(-0.0510216505388318,0.106149619882943,
-0.0164977839420939));
#17740=CARTESIAN_POINT('Ctrl Pts',(-0.0863355867949722,0.0891756983861136,
-0.0138503945678339));
#17741=CARTESIAN_POINT('Ctrl Pts',(-0.13808023131828,0.0175094743621551,
-0.00855561581931395));
#17742=CARTESIAN_POINT('Ctrl Pts',(-0.0894531427980795,-0.106808298616542,
-0.000613447696533924));
#17743=CARTESIAN_POINT('Ctrl Pts',(0.0412394829729132,-0.132934609947913,
0.00732872042624606));
#17744=CARTESIAN_POINT('Ctrl Pts',(0.134092250525203,-0.0374520209666004,
0.0152708885490261));
#17745=CARTESIAN_POINT('Ctrl Pts',(0.104134301645602,0.0924305194826295,
0.023213056671806));
#17746=CARTESIAN_POINT('Ctrl Pts',(-0.0212379681243542,0.137589894578696,
0.0311552247945861));
#17747=CARTESIAN_POINT('Ctrl Pts',(-0.127145335141994,0.0567276974868182,
0.039097392917366));
#17748=CARTESIAN_POINT('Ctrl Pts',(-0.116579117211717,-0.0761160149501382,
0.0470395610401461));
#17749=CARTESIAN_POINT('Ctrl Pts',(0.000787973702835166,-0.139222729671589,
0.054981729162926));
#17750=CARTESIAN_POINT('Ctrl Pts',(0.117431922513572,-0.0747907597173192,
0.0629238972857061));
#17751=CARTESIAN_POINT('Ctrl Pts',(0.126496838785129,0.0581591461343325,
0.070866065408486));
#17752=CARTESIAN_POINT('Ctrl Pts',(0.0196773008918215,0.137828289815661,
0.0788082335312661));
#17753=CARTESIAN_POINT('Ctrl Pts',(-0.105168479521776,0.0912330920368172,
0.0867504016540459));
#17754=CARTESIAN_POINT('Ctrl Pts',(-0.133669226619255,-0.0389412707994331,
0.0946925697768262));
#17755=CARTESIAN_POINT('Ctrl Pts',(-0.0397151780004399,-0.133441281507892,
0.102634737899606));
#17756=CARTESIAN_POINT('Ctrl Pts',(0.0906220264938673,-0.105695447092796,
0.110576906022386));
#17757=CARTESIAN_POINT('Ctrl Pts',(0.137940159127448,0.0188783162799928,
0.118519074145166));
#17758=CARTESIAN_POINT('Ctrl Pts',(0.0588909273047484,0.126157580947307,
0.126461242267946));
#17759=CARTESIAN_POINT('Ctrl Pts',(-0.074108440039672,0.117863552156501,
0.134403410390726));
#17760=CARTESIAN_POINT('Ctrl Pts',(-0.139216864956951,0.00159439502933392,
0.142345578513506));
#17761=CARTESIAN_POINT('Ctrl Pts',(-0.0767883381764272,-0.116135388594389,
0.150287746636286));
#17762=CARTESIAN_POINT('Ctrl Pts',(0.0559861945572589,-0.127473226882309,
0.158229914759066));
#17763=CARTESIAN_POINT('Ctrl Pts',(0.137471621702818,-0.0220324926503626,
0.166172082881846));
#17764=CARTESIAN_POINT('Ctrl Pts',(0.0930189202108026,0.103592267873211,
0.174114251004626));
#17765=CARTESIAN_POINT('Ctrl Pts',(-0.0366486683060043,0.134315868829211,
0.182056419127406));
#17766=CARTESIAN_POINT('Ctrl Pts',(-0.132742311638566,0.0419923350165386,
0.189998587250186));
#17767=CARTESIAN_POINT('Ctrl Pts',(-0.107230360350792,-0.0888004916405464,
0.197940755372966));
#17768=CARTESIAN_POINT('Ctrl Pts',(0.0165156171993534,-0.138242945169174,
0.205882923495746));
#17769=CARTESIAN_POINT('Ctrl Pts',(0.125131592687617,-0.061040658666823,
0.213825091618526));
#17770=CARTESIAN_POINT('Ctrl Pts',(0.119114174013628,0.0720811421096423,
0.221767259741306));
#17771=CARTESIAN_POINT('Ctrl Pts',(0.0039759348809324,0.139169211541763,
0.229709427864086));
#17772=CARTESIAN_POINT('Ctrl Pts',(-0.114804669066963,0.0787639858025777,
0.237651595986866));
#17773=CARTESIAN_POINT('Ctrl Pts',(-0.128412401817242,-0.0537971426620367,
0.245593764109646));
#17774=CARTESIAN_POINT('Ctrl Pts',(-0.024381182195918,-0.137074561658528,
0.253535932232426));
#17775=CARTESIAN_POINT('Ctrl Pts',(0.101985705091022,-0.094777599970642,
0.261478100355206));
#17776=CARTESIAN_POINT('Ctrl Pts',(0.134923209124943,0.0343453801629359,
0.269420268477986));
#17777=CARTESIAN_POINT('Ctrl Pts',(0.0442571924125319,0.132004463632409,
0.277362436600766));
#17778=CARTESIAN_POINT('Ctrl Pts',(-0.0869529592639067,0.108733897080731,
0.285304604723546));
#17779=CARTESIAN_POINT('Ctrl Pts',(-0.138505267237684,-0.0141480898545381,
0.293246772846326));
#17780=CARTESIAN_POINT('Ctrl Pts',(-0.0631725212350128,-0.124068972994571,
0.301188940969106));
#17781=CARTESIAN_POINT('Ctrl Pts',(0.0700327441786229,-0.12032993078169,
0.309131109091886));
#17782=CARTESIAN_POINT('Ctrl Pts',(0.139080821187468,-0.00635631000930847,
0.317073277214666));
#17783=CARTESIAN_POINT('Ctrl Pts',(0.0807165776729536,0.11344034374014,
0.325015445337446));
#17784=CARTESIAN_POINT('Ctrl Pts',(-0.0515923433190751,0.129313988454311,
0.332957613460226));
#17785=CARTESIAN_POINT('Ctrl Pts',(-0.136637377548019,0.026722734813544,
0.340899781583006));
#17786=CARTESIAN_POINT('Ctrl Pts',(-0.0965085366518414,-0.100349289247285,
0.348841949705786));
#17787=CARTESIAN_POINT('Ctrl Pts',(0.0320320385160992,-0.135491055083419,
0.356784117828566));
#17788=CARTESIAN_POINT('Ctrl Pts',(0.131227975626944,-0.0465090949381858,
0.364726285951346));
#17789=CARTESIAN_POINT('Ctrl Pts',(0.110205605501345,0.0850799742312894,
0.372668454074126));
#17790=CARTESIAN_POINT('Ctrl Pts',(-0.0117764211155082,0.138727046407055,
0.380610622196906));
#17791=CARTESIAN_POINT('Ctrl Pts',(-0.122970036152848,0.065285892102983,
0.388552790319686));
#17792=CARTESIAN_POINT('Ctrl Pts',(-0.121510464882371,-0.0679638464419502,
0.396494958442466));
#17793=CARTESIAN_POINT('Ctrl Pts',(-0.00873482453528946,-0.138951719454826,
0.404437126565246));
#17794=CARTESIAN_POINT('Ctrl Pts',(0.112042812448737,-0.0826455423945668,
0.412379294688026));
#17795=CARTESIAN_POINT('Ctrl Pts',(0.130177722634257,0.049372441998279,
0.420321462810806));
#17796=CARTESIAN_POINT('Ctrl Pts',(0.0290564652212241,0.136160197297018,
0.428263630933586));
#17797=CARTESIAN_POINT('Ctrl Pts',(-0.098683499418539,0.098211223603141,
0.436205799056366));
#17798=CARTESIAN_POINT('Ctrl Pts',(-0.136019240449831,-0.0297093205335648,
0.444147967179146));
#17799=CARTESIAN_POINT('Ctrl Pts',(-0.0487473834415776,-0.130413074907061,
0.452090135301926));
#17800=CARTESIAN_POINT('Ctrl Pts',(0.0831820848081396,-0.111645054821459,
0.460032303424706));
#17801=CARTESIAN_POINT('Ctrl Pts',(0.138908217753341,0.00940130521287039,
0.467974471547486));
#17802=CARTESIAN_POINT('Ctrl Pts',(0.0673801526530663,0.121835103839429,
0.475916639670265));
#17803=CARTESIAN_POINT('Ctrl Pts',(-0.0658750545035054,0.12265543075329,
0.483858807793047));
#17804=CARTESIAN_POINT('Ctrl Pts',(-0.138781944133385,0.0111107822259715,
0.491800975915825));
#17805=CARTESIAN_POINT('Ctrl Pts',(-0.084550315326251,-0.110612484274364,
0.499743144038607));
#17806=CARTESIAN_POINT('Ctrl Pts',(0.0471380885036503,-0.131003351527116,
0.507685312161385));
#17807=CARTESIAN_POINT('Ctrl Pts',(0.135643160584381,-0.031381690295376,
0.515627480284167));
#17808=CARTESIAN_POINT('Ctrl Pts',(0.0998851624184703,0.0969888232104648,
0.523569648406945));
#17809=CARTESIAN_POINT('Ctrl Pts',(-0.0273779061153799,0.136507610615132,
0.531511816529727));
#17810=CARTESIAN_POINT('Ctrl Pts',(-0.129560000008381,0.0509714027366644,
0.539453984652505));
#17811=CARTESIAN_POINT('Ctrl Pts',(-0.113051823689188,-0.0812598465397498,
0.547396152775286));
#17812=CARTESIAN_POINT('Ctrl Pts',(0.00702343738442799,-0.139048728244533,
0.555338320898066));
#17813=CARTESIAN_POINT('Ctrl Pts',(0.12066450826877,-0.0694546898587181,
0.563280489020846));
#17814=CARTESIAN_POINT('Ctrl Pts',(0.123764493242992,0.063766979789076,
0.571222657143626));
#17815=CARTESIAN_POINT('Ctrl Pts',(0.0134834875971477,0.13857154491934,
0.579164825266405));
#17816=CARTESIAN_POINT('Ctrl Pts',(-0.109149777898995,0.0864303389077871,
0.587106993389186));
#17817=CARTESIAN_POINT('Ctrl Pts',(-0.131790633456927,-0.0448899368693808,
0.595049161511966));
#17818=CARTESIAN_POINT('Ctrl Pts',(-0.0336977294021144,-0.135086418755761,
0.602991329634746));
#17819=CARTESIAN_POINT('Ctrl Pts',(0.0952657566843092,-0.101529863106778,
0.610933497757526));
#17820=CARTESIAN_POINT('Ctrl Pts',(0.136956022624868,0.025038477707157,
0.618875665880307));
#17821=CARTESIAN_POINT('Ctrl Pts',(0.0531805018142573,0.128669000640787,
0.626817834003085));
#17822=CARTESIAN_POINT('Ctrl Pts',(-0.0793138220987445,0.114425500318782,
0.634760002125867));
#17823=CARTESIAN_POINT('Ctrl Pts',(-0.139148536750765,-0.00464351367351466,
0.642702170248646));
#17824=CARTESIAN_POINT('Ctrl Pts',(-0.0715088964667609,-0.119458592094588,
0.650644338371427));
#17825=CARTESIAN_POINT('Ctrl Pts',(0.0616402393688536,-0.124837327709565,
0.658586506494205));
#17826=CARTESIAN_POINT('Ctrl Pts',(0.138320583400205,-0.0158522461166236,
0.666528674616987));
#17827=CARTESIAN_POINT('Ctrl Pts',(0.0882850628235238,0.107655121482266,
0.674470842739765));
#17828=CARTESIAN_POINT('Ctrl Pts',(-0.0426286451686149,0.132539337972556,
0.682413010862546));
#17829=CARTESIAN_POINT('Ctrl Pts',(-0.13449013477919,0.0360039045964495,
0.690355178985326));
#17830=CARTESIAN_POINT('Ctrl Pts',(-0.103144844235522,-0.0935148042116587,
0.698297347108106));
#17831=CARTESIAN_POINT('Ctrl Pts',(0.022691720100341,-0.137364345221032,
0.706239515230886));
#17832=CARTESIAN_POINT('Ctrl Pts',(0.127740337615313,-0.0553740340325759,
0.714181683353665));
#17833=CARTESIAN_POINT('Ctrl Pts',(0.115765682611161,0.077344581120379,
0.722123851476446));
#17834=CARTESIAN_POINT('Ctrl Pts',(-0.00226223072526165,0.139207614056346,
0.730066019599226));
#17835=CARTESIAN_POINT('Ctrl Pts',(-0.118217708309552,0.0735421711751344,
0.738008187722006));
#17836=CARTESIAN_POINT('Ctrl Pts',(-0.125873620115675,-0.059495455776806,
0.745950355844786));
#17837=CARTESIAN_POINT('Ctrl Pts',(-0.0182163644075178,-0.138029133036789,
0.753892523967566));
#17838=CARTESIAN_POINT('Ctrl Pts',(0.106128952536144,-0.0901139441634624,
0.761834692090347));
#17839=CARTESIAN_POINT('Ctrl Pts',(0.133249245915149,0.0403548753208232,
0.769776860213125));
#17840=CARTESIAN_POINT('Ctrl Pts',(0.0382995408207276,0.133854483197375,
0.777719028335907));
#17841=CARTESIAN_POINT('Ctrl Pts',(-0.0917364783268051,0.104729633071593,
0.785661196458685));
#17842=CARTESIAN_POINT('Ctrl Pts',(-0.137732458880487,-0.0203383202317681,
0.793603364581467));
#17843=CARTESIAN_POINT('Ctrl Pts',(-0.0575513573065257,-0.126774282767806,
0.801545532704245));
#17844=CARTESIAN_POINT('Ctrl Pts',(0.0753527000357912,-0.117071978271622,
0.809487700827026));
#17845=CARTESIAN_POINT('Ctrl Pts',(0.139225942868322,-0.000119714417332432,
0.817429868949805));
#17846=CARTESIAN_POINT('Ctrl Pts',(0.0755539188089132,0.116942220141962,
0.825372037072586));
#17847=CARTESIAN_POINT('Ctrl Pts',(-0.0573332568284509,0.12687306712048,
0.833314205195366));
#17848=CARTESIAN_POINT('Ctrl Pts',(-0.13769727914169,0.0205751504512258,
0.841256373318145));
#17849=CARTESIAN_POINT('Ctrl Pts',(-0.0919164475821765,-0.104571717796869,
0.849198541440926));
#17850=CARTESIAN_POINT('Ctrl Pts',(0.0380692928980519,-0.133920149482284,
0.857140709563706));
#17851=CARTESIAN_POINT('Ctrl Pts',(0.133179650076608,-0.0405839661022353,
0.865082877686486));
#17852=CARTESIAN_POINT('Ctrl Pts',(0.106283765719693,0.0899312995767124,
0.873025045809266));
#17853=CARTESIAN_POINT('Ctrl Pts',(-0.0179789669825735,0.138060255849953,
0.880967213932046));
#17854=CARTESIAN_POINT('Ctrl Pts',(-0.125771118879347,0.0597118342956578,
0.888909382054826));
#17855=CARTESIAN_POINT('Ctrl Pts',(-0.118344004924669,-0.0733387619032726,
0.896851550177606));
#17856=CARTESIAN_POINT('Ctrl Pts',(-0.00250162451743248,-0.139203517821528,
0.904793718300386));
#17857=CARTESIAN_POINT('Ctrl Pts',(0.115632500949424,-0.0775435504945224,
0.912735886423165));
#17858=CARTESIAN_POINT('Ctrl Pts',(0.127835376168433,0.0551542754370876,
0.920678054545947));
#17859=CARTESIAN_POINT('Ctrl Pts',(0.0229279137899797,0.137325118854324,
0.928620222668725));
#17860=CARTESIAN_POINT('Ctrl Pts',(-0.102983873094174,0.0936920454555137,
0.936562390791507));
#17861=CARTESIAN_POINT('Ctrl Pts',(-0.134551852288801,-0.0357725669300891,
0.944504558914285));
#17862=CARTESIAN_POINT('Ctrl Pts',(-0.0428565117498991,-0.132465832952297,
0.952446727037066));
#17863=CARTESIAN_POINT('Ctrl Pts',(0.0880997963686447,-0.107806787258123,
0.960388895159846));
#17864=CARTESIAN_POINT('Ctrl Pts',(0.138347640177547,0.0156143509765511,
0.968331063282625));
#17865=CARTESIAN_POINT('Ctrl Pts',(0.061854832590724,0.124731139593481,
0.976273231405407));
#17866=CARTESIAN_POINT('Ctrl Pts',(-0.0713033562375951,0.119581390225944,
0.984215399528185));
#17867=CARTESIAN_POINT('Ctrl Pts',(-0.139140345480169,0.00488280234845834,
0.992157567650966));
#17868=CARTESIAN_POINT('Ctrl Pts',(-0.0795104838321055,-0.114288934109561,
1.00009973577375));
#17869=CARTESIAN_POINT('Ctrl Pts',(0.0529591494285269,-0.128760265574912,
1.00804190389653));
#17870=CARTESIAN_POINT('Ctrl Pts',(0.136912761112491,-0.0252739657289669,
1.0159840720193));
#17871=CARTESIAN_POINT('Ctrl Pts',(0.0954402180350474,0.101365883217864,
1.02392624014209));
#17872=CARTESIAN_POINT('Ctrl Pts',(-0.0334653697086341,0.135144169424284,
1.03186840826486));
#17873=CARTESIAN_POINT('Ctrl Pts',(-0.131713240771149,0.0451165125500212,
1.03981057638765));
#17874=CARTESIAN_POINT('Ctrl Pts',(-0.109298251871946,-0.0862425048155002,
1.04775274451043));
#17875=CARTESIAN_POINT('Ctrl Pts',(0.0132451643780021,-0.13859452774087,
1.05569491263321));
#17876=CARTESIAN_POINT('Ctrl Pts',(0.123654649330263,-0.0639797248987874,
1.06363708075599));
#17877=CARTESIAN_POINT('Ctrl Pts',(0.120783771971213,0.0692470788374567,
1.07157924887876));
#17878=CARTESIAN_POINT('Ctrl Pts',(0.00726255089817806,0.139036444335888,
1.07952141700155));
#17879=CARTESIAN_POINT('Ctrl Pts',(-0.112911912907791,0.0814541430660127,
1.08746358512433));
#17880=CARTESIAN_POINT('Ctrl Pts',(-0.129647464608677,-0.0507485213543897,
1.09540575324711));
#17881=CARTESIAN_POINT('Ctrl Pts',(-0.0276126195379174,-0.136460326620484,
1.10334792136989));
#17882=CARTESIAN_POINT('Ctrl Pts',(0.0997182217817603,-0.0971604536002107,
1.11129008949267));
#17883=CARTESIAN_POINT('Ctrl Pts',(0.135696927507188,0.0311483765905046,
1.11923225761545));
#17884=CARTESIAN_POINT('Ctrl Pts',(0.0473633069609982,0.130922093830007,
1.12717442573822));
#17885=CARTESIAN_POINT('Ctrl Pts',(-0.0843599685788644,0.110757722983492,
1.13511659386101));
#17886=CARTESIAN_POINT('Ctrl Pts',(-0.138800846271631,-0.0108721006891078,
1.14305876198379));
#17887=CARTESIAN_POINT('Ctrl Pts',(-0.0660858892268601,-0.122541963197144,
1.15100093010657));
#17888=CARTESIAN_POINT('Ctrl Pts',(0.0671705316110708,-0.121950798202395,
1.15894309822935));
#17889=CARTESIAN_POINT('Ctrl Pts',(0.138891844802359,-0.00964017357273747,
1.16688526635212));
#17890=CARTESIAN_POINT('Ctrl Pts',(0.0833739592533277,0.111501840422208,
1.17482743447491));
#17891=CARTESIAN_POINT('Ctrl Pts',(-0.0485230383040216,0.130496713571114,
1.18276960259768));
#17892=CARTESIAN_POINT('Ctrl Pts',(-0.135967947813762,0.0299431906521225,
1.19071177072047));
#17893=CARTESIAN_POINT('Ctrl Pts',(-0.0988522486080867,-0.0980413710850678,
1.19865393884324));
#17894=CARTESIAN_POINT('Ctrl Pts',(0.0288222657999454,-0.136209964735594,
1.20659610696603));
#17895=CARTESIAN_POINT('Ctrl Pts',(0.130092623711363,-0.0495962373069701,
1.21453827508881));
#17896=CARTESIAN_POINT('Ctrl Pts',(0.112184773380136,0.082452738709893,
1.22248044321158));
#17897=CARTESIAN_POINT('Ctrl Pts',(-0.00849585454694533,0.138966535376798,
1.23042261133437));
#17898=CARTESIAN_POINT('Ctrl Pts',(-0.121393406896754,0.0681727090639588,
1.23836477945715));
#17899=CARTESIAN_POINT('Ctrl Pts',(-0.123082127310551,-0.0650743223999996,
1.24630694757992));
#17900=CARTESIAN_POINT('Ctrl Pts',(-0.0120149744006178,-0.138706589206355,
1.25424911570271));
#17901=CARTESIAN_POINT('Ctrl Pts',(0.110059129405696,-0.0852693704304675,
1.26219128382548));
#17902=CARTESIAN_POINT('Ctrl Pts',(0.13130776387206,0.0462833517151888,
1.27013345194827));
#17903=CARTESIAN_POINT('Ctrl Pts',(0.0322649968732001,0.135435768819968,
1.27807562007105));
#17904=CARTESIAN_POINT('Ctrl Pts',(-0.0963358219719167,0.100515107841202,
1.28601778819382));
#17905=CARTESIAN_POINT('Ctrl Pts',(-0.136683130933199,-0.0264877182308561,
1.29395995631661));
#17906=CARTESIAN_POINT('Ctrl Pts',(-0.0518146499729274,-0.129225073214149,
1.30190212443939));
#17907=CARTESIAN_POINT('Ctrl Pts',(0.0805213734929343,-0.11357898534207,
1.30984429256217));
#17908=CARTESIAN_POINT('Ctrl Pts',(0.1390915465469,0.0061171215252809,1.31778646068495));
#17909=CARTESIAN_POINT('Ctrl Pts',(0.0702395735793815,0.120209316621791,
1.32572862880773));
#17910=CARTESIAN_POINT('Ctrl Pts',(-0.0629590648350173,0.124177428154433,
1.33367079693051));
#17911=CARTESIAN_POINT('Ctrl Pts',(-0.138480731711197,0.0143862582011507,
1.34161296505328));
#17912=CARTESIAN_POINT('Ctrl Pts',(-0.0871398218994898,-0.108584202098263,
1.34955513317607));
#17913=CARTESIAN_POINT('Ctrl Pts',(0.0440301174146577,-0.132080378229483,
1.35749730129884));
#17914=CARTESIAN_POINT('Ctrl Pts',(0.13486394497766,-0.0345773583278084,
1.36543946942163));
#17915=CARTESIAN_POINT('Ctrl Pts',(0.102148545386143,0.0946020732301706,
1.3733816375444));
#17916=CARTESIAN_POINT('Ctrl Pts',(-0.0241454188302812,0.137116288461919,
1.38132380566719));
#17917=CARTESIAN_POINT('Ctrl Pts',(-0.128319693277533,0.0540178939468163,
1.38926597378996));
#17918=CARTESIAN_POINT('Ctrl Pts',(-0.114939956470138,-0.0785664351508689,
1.39720814191275));
#17919=CARTESIAN_POINT('Ctrl Pts',(0.00373660876362508,-0.139175849115243,
1.40515031003553));
#17920=CARTESIAN_POINT('Ctrl Pts',(0.118990018389619,-0.0722858665142316,
1.41309247815831));
#17921=CARTESIAN_POINT('Ctrl Pts',(0.125236419206141,0.0608253567263532,
1.42103464628109));
#17922=CARTESIAN_POINT('Ctrl Pts',(0.0167532566496359,0.13821437898841,
1.42897681440387));
#17923=CARTESIAN_POINT('Ctrl Pts',(-0.107077349343502,0.0889846891406984,
1.43691898252665));
#17924=CARTESIAN_POINT('Ctrl Pts',(-0.132814597987359,-0.0417638487589672,
1.44486115064943));
#17925=CARTESIAN_POINT('Ctrl Pts',(-0.0368790902657646,-0.134252921254984,
1.45280331877221));
#17926=CARTESIAN_POINT('Ctrl Pts',(0.0928396680879532,-0.103751556080299,
1.46074548689499));
#17927=CARTESIAN_POINT('Ctrl Pts',(0.137511141307062,0.0217950526079239,
1.46868765501776));
#17928=CARTESIAN_POINT('Ctrl Pts',(0.0562018483347667,0.127378648737854,
1.47662982314055));
#17929=CARTESIAN_POINT('Ctrl Pts',(-0.0765818961642769,0.116263681173923,
1.48457199126332));
#17930=CARTESIAN_POINT('Ctrl Pts',(-0.13923195096087,-0.00134816270381636,
1.49251415938611));
#17931=CARTESIAN_POINT('Ctrl Pts',(-0.0742871760264013,-0.117748889605885,
1.50045632750888));
#17932=CARTESIAN_POINT('Ctrl Pts',(0.0586284551779338,-0.126233948370975,
1.50839849563167));
#17933=CARTESIAN_POINT('Ctrl Pts',(0.137995068118234,-0.019163470063063,
1.51634066375444));
#17934=CARTESIAN_POINT('Ctrl Pts',(0.0906261803825392,0.105639137646141,
1.52428283187723));
#17935=CARTESIAN_POINT('Ctrl Pts',(0.00417072711528833,0.124051375507138,
1.52957761062575));
#17936=CARTESIAN_POINT('Ctrl Pts',(-0.0334019664627544,0.1129391839063,
1.53222500000001));
#17937=CARTESIAN_POINT('Ctrl Pts',(-0.0551480035117261,0.114734422509858,
-0.0109985226280628));
#17938=CARTESIAN_POINT('Ctrl Pts',(-0.093317938433455,0.0963877427684319,
-0.00835113325380276));
#17939=CARTESIAN_POINT('Ctrl Pts',(-0.149247407742026,0.0189255452031589,
-0.00305635450528277));
#17940=CARTESIAN_POINT('Ctrl Pts',(-0.0966876253720675,-0.115446371588928,
0.00488581361749726));
#17941=CARTESIAN_POINT('Ctrl Pts',(0.0445747075563756,-0.143685636564375,
0.0128279817402772));
#17942=CARTESIAN_POINT('Ctrl Pts',(0.144936900801175,-0.0404809362687151,
0.0207701498630572));
#17943=CARTESIAN_POINT('Ctrl Pts',(0.112556116319125,0.0999057960529736,
0.0287123179858373));
#17944=CARTESIAN_POINT('Ctrl Pts',(-0.0229555792165621,0.148717415239805,
0.0366544861086172));
#17945=CARTESIAN_POINT('Ctrl Pts',(-0.137428156769908,0.0613155244327884,
0.0445966542313972));
#17946=CARTESIAN_POINT('Ctrl Pts',(-0.126007400730642,-0.0822718633254329,
0.0525388223541772));
#17947=CARTESIAN_POINT('Ctrl Pts',(0.000851700720621877,-0.150482305134309,
0.0604809904769572));
#17948=CARTESIAN_POINT('Ctrl Pts',(0.126929176276611,-0.0808394286734405,
0.0684231585997372));
#17949=CARTESIAN_POINT('Ctrl Pts',(0.136727213562698,0.0628627408439891,
0.0763653267225173));
#17950=CARTESIAN_POINT('Ctrl Pts',(0.0212686937255662,0.148975090584026,
0.0843074948452972));
#17951=CARTESIAN_POINT('Ctrl Pts',(-0.113673932864549,0.0986115272026031,
0.0922496629680772));
#17952=CARTESIAN_POINT('Ctrl Pts',(-0.144479665027646,-0.0420906285100245,
0.100191831090857));
#17953=CARTESIAN_POINT('Ctrl Pts',(-0.0429271251068198,-0.144233284958223,
0.108133999213637));
#17954=CARTESIAN_POINT('Ctrl Pts',(0.0979510420095061,-0.114243518700172,
0.116076167336417));
#17955=CARTESIAN_POINT('Ctrl Pts',(0.149096007275942,0.0204050915936607,
0.124018335459197));
#17956=CARTESIAN_POINT('Ctrl Pts',(0.0636537044864716,0.136360518400275,
0.131960503581977));
#17957=CARTESIAN_POINT('Ctrl Pts',(-0.0801019266996435,0.127395713772213,
0.139902671704757));
#17958=CARTESIAN_POINT('Ctrl Pts',(-0.15047596611352,0.00172334100814176,
0.147844839827537));
#17959=CARTESIAN_POINT('Ctrl Pts',(-0.0829985603893774,-0.125527785761544,
0.155787007950317));
#17960=CARTESIAN_POINT('Ctrl Pts',(0.0605140527882773,-0.137782566606816,
0.163729176073097));
#17961=CARTESIAN_POINT('Ctrl Pts',(0.148589577098441,-0.0238143605552183,
0.171671344195877));
#17962=CARTESIAN_POINT('Ctrl Pts',(0.100541783424623,0.111970245809892,
0.179613512318657));
#17963=CARTESIAN_POINT('Ctrl Pts',(-0.0396126128240685,0.145178604134651,
0.187555680441437));
#17964=CARTESIAN_POINT('Ctrl Pts',(-0.143477786216001,0.0453884461694337,
0.195497848564217));
#17965=CARTESIAN_POINT('Ctrl Pts',(-0.115902567375552,-0.095982191346566,
0.203440016686997));
#17966=CARTESIAN_POINT('Ctrl Pts',(0.0178513102906219,-0.149423281002214,
0.211382184809777));
#17967=CARTESIAN_POINT('Ctrl Pts',(0.135251553802876,-0.0659772944027704,
0.219324352932557));
#17968=CARTESIAN_POINT('Ctrl Pts',(0.128747479107914,0.07791067196398,0.227266521055337));
#17969=CARTESIAN_POINT('Ctrl Pts',(0.00429748682099232,0.150424458749874,
0.235208689178117));
#17970=CARTESIAN_POINT('Ctrl Pts',(-0.124089444892588,0.0851339876261335,
0.243150857300897));
#17971=CARTESIAN_POINT('Ctrl Pts',(-0.138797696890977,-0.0581479623084488,
0.251093025423677));
#17972=CARTESIAN_POINT('Ctrl Pts',(-0.0263529993083425,-0.148160405002171,
0.259035193546457));
#17973=CARTESIAN_POINT('Ctrl Pts',(0.110233752987369,-0.102442695616748,
0.266977361669237));
#17974=CARTESIAN_POINT('Ctrl Pts',(0.145835062802846,0.0371230472913779,
0.274919529792017));
#17975=CARTESIAN_POINT('Ctrl Pts',(0.0478364728857143,0.142680265085169,
0.282861697914797));
#17976=CARTESIAN_POINT('Ctrl Pts',(-0.0939852406223356,0.117527701960322,
0.290803866037577));
#17977=CARTESIAN_POINT('Ctrl Pts',(-0.14970681824969,-0.01529231023972,
0.298746034160357));
#17978=CARTESIAN_POINT('Ctrl Pts',(-0.0682815703945392,-0.134102995221473,
0.306688202283137));
#17979=CARTESIAN_POINT('Ctrl Pts',(0.0756966107742644,-0.1300615596562,
0.314630370405917));
#17980=CARTESIAN_POINT('Ctrl Pts',(0.150328919865546,-0.00687037371415525,
0.322572538528697));
#17981=CARTESIAN_POINT('Ctrl Pts',(0.0872444944832666,0.122614780370367,
0.330514706651477));
#17982=CARTESIAN_POINT('Ctrl Pts',(-0.0557648508131485,0.139772198940638,
0.338456874774257));
#17983=CARTESIAN_POINT('Ctrl Pts',(-0.147687863823926,0.0288839239377102,
0.346399042897038));
#17984=CARTESIAN_POINT('Ctrl Pts',(-0.104313621021262,-0.10846499275041,
0.354341211019817));
#17985=CARTESIAN_POINT('Ctrl Pts',(0.0346226151823369,-0.146448833047075,
0.362283379142597));
#17986=CARTESIAN_POINT('Ctrl Pts',(0.141840978962514,-0.0502704970123603,
0.370225547265377));
#17987=CARTESIAN_POINT('Ctrl Pts',(0.119118434135606,0.0919607787700563,
0.378167715388157));
#17988=CARTESIAN_POINT('Ctrl Pts',(-0.0127288338612142,0.149946533709345,
0.386109883510937));
#17989=CARTESIAN_POINT('Ctrl Pts',(-0.132915182358376,0.070565859178174,
0.394052051633717));
#17990=CARTESIAN_POINT('Ctrl Pts',(-0.131337568919768,-0.0734603918663599,
0.401994219756497));
#17991=CARTESIAN_POINT('Ctrl Pts',(-0.00944124952954395,-0.150189377088511,
0.409936387879277));
#17992=CARTESIAN_POINT('Ctrl Pts',(0.121104224366159,-0.0893294633566384,
0.417878556002057));
#17993=CARTESIAN_POINT('Ctrl Pts',(0.140705787232781,0.0533654159743681,
0.425820724124838));
#17994=CARTESIAN_POINT('Ctrl Pts',(0.0314063937394313,0.147172091835368,
0.433762892247617));
#17995=CARTESIAN_POINT('Ctrl Pts',(-0.106664482920656,0.106154012011714,
0.441705060370398));
#17996=CARTESIAN_POINT('Ctrl Pts',(-0.147019735166745,-0.032112048430678,
0.449647228493177));
#17997=CARTESIAN_POINT('Ctrl Pts',(-0.052689806088835,-0.14096017351449,
0.457589396615958));
#17998=CARTESIAN_POINT('Ctrl Pts',(0.0899093983958942,-0.120674298270189,
0.465531564738737));
#17999=CARTESIAN_POINT('Ctrl Pts',(0.15014235720654,0.0101616315312987,
0.473473732861518));
#18000=CARTESIAN_POINT('Ctrl Pts',(0.0728294921055832,0.131688462906045,
0.481415900984297));
#18001=CARTESIAN_POINT('Ctrl Pts',(-0.071202669822089,0.132575133389036,
0.489358069107078));
#18002=CARTESIAN_POINT('Ctrl Pts',(-0.150005871264529,0.012009361726732,
0.497300237229857));
#18003=CARTESIAN_POINT('Ctrl Pts',(-0.0913882839399832,-0.119558219045865,
0.505242405352637));
#18004=CARTESIAN_POINT('Ctrl Pts',(0.0509503601487159,-0.141598188489932,
0.513184573475417));
#18005=CARTESIAN_POINT('Ctrl Pts',(0.146613240011817,-0.0339196703426114,
0.521126741598197));
#18006=CARTESIAN_POINT('Ctrl Pts',(0.107963329873666,0.104832750538675,
0.529068909720978));
#18007=CARTESIAN_POINT('Ctrl Pts',(-0.0295920819230583,0.147547602048875,
0.537011077843756));
#18008=CARTESIAN_POINT('Ctrl Pts',(-0.140038106568177,0.055093691941219,
0.544953245966537));
#18009=CARTESIAN_POINT('Ctrl Pts',(-0.122194838935542,-0.0878316999746162,
0.552895414089317));
#18010=CARTESIAN_POINT('Ctrl Pts',(0.00759145471482065,-0.150294231420327,
0.560837582212097));
#18011=CARTESIAN_POINT('Ctrl Pts',(0.130423195946632,-0.0750718065719766,
0.568779750334878));
#18012=CARTESIAN_POINT('Ctrl Pts',(0.133773890807325,0.0689241055160235,
0.576721918457657));
#18013=CARTESIAN_POINT('Ctrl Pts',(0.0145739585745413,0.149778456108953,
0.584664086580438));
#18014=CARTESIAN_POINT('Ctrl Pts',(-0.117977216952174,0.0934203535806499,
0.592606254703216));
#18015=CARTESIAN_POINT('Ctrl Pts',(-0.142449141490696,-0.0485203902651028,
0.600548422825998));
#18016=CARTESIAN_POINT('Ctrl Pts',(-0.036423018067407,-0.146011471938939,
0.608490590948776));
#18017=CARTESIAN_POINT('Ctrl Pts',(0.102970331784443,-0.109741044988262,
0.616432759071558));
#18018=CARTESIAN_POINT('Ctrl Pts',(0.148032279177632,0.0270634532975707,
0.624374927194337));
#18019=CARTESIAN_POINT('Ctrl Pts',(0.0574814509102497,0.139075048028633,
0.632317095317117));
#18020=CARTESIAN_POINT('Ctrl Pts',(-0.0857282916847416,0.123679611042927,
0.640259263439898));
#18021=CARTESIAN_POINT('Ctrl Pts',(-0.150402111894479,-0.00501905574730406,
0.648201431562677));
#18022=CARTESIAN_POINT('Ctrl Pts',(-0.0772921462128499,-0.129119751845818,
0.656143599685457));
#18023=CARTESIAN_POINT('Ctrl Pts',(0.0666253659236285,-0.134933490277457,
0.664085767808237));
#18024=CARTESIAN_POINT('Ctrl Pts',(0.14950719819016,-0.0171342893707992,
0.672027935931017));
#18025=CARTESIAN_POINT('Ctrl Pts',(0.0954250774564579,0.11636168087194,
0.679970104053797));
#18026=CARTESIAN_POINT('Ctrl Pts',(-0.0460762176180427,0.143258397146306,
0.687912272176577));
#18027=CARTESIAN_POINT('Ctrl Pts',(-0.145366963764729,0.0389157041403328,
0.695854440299358));
#18028=CARTESIAN_POINT('Ctrl Pts',(-0.111486636987321,-0.101077771820372,
0.703796608422136));
#18029=CARTESIAN_POINT('Ctrl Pts',(0.02452690272786,-0.148473624679578,
0.711738776544918));
#18030=CARTESIAN_POINT('Ctrl Pts',(0.138071279799868,-0.0598523840572839,
0.719680944667696));
#18031=CARTESIAN_POINT('Ctrl Pts',(0.125128179973684,0.0835997892305201,
0.727623112790477));
#18032=CARTESIAN_POINT('Ctrl Pts',(-0.00244518761474098,0.150465967050502,
0.735565280913257));
#18033=CARTESIAN_POINT('Ctrl Pts',(-0.127778512144395,0.0794898610961098,
0.743507449036036));
#18034=CARTESIAN_POINT('Ctrl Pts',(-0.136053592364468,-0.0643071239260258,
0.751449617158818));
#18035=CARTESIAN_POINT('Ctrl Pts',(-0.019689604662082,-0.149192176910068,
0.759391785281597));
#18036=CARTESIAN_POINT('Ctrl Pts',(0.114712083700712,-0.0974018687498071,
0.767333953404378));
#18037=CARTESIAN_POINT('Ctrl Pts',(0.144025718573537,0.0436185576594447,
0.775276121527157));
#18038=CARTESIAN_POINT('Ctrl Pts',(0.0413969989087525,0.14467990414796,
0.783218289649938));
#18039=CARTESIAN_POINT('Ctrl Pts',(-0.0991556246317344,0.113199594905656,
0.791160457772717));
#18040=CARTESIAN_POINT('Ctrl Pts',(-0.148871509365196,-0.021983172706469,
0.799102625895497));
#18041=CARTESIAN_POINT('Ctrl Pts',(-0.062205797368885,-0.137027095702329,
0.807044794018277));
#18042=CARTESIAN_POINT('Ctrl Pts',(0.081446815661698,-0.126540121706451,
0.814986962141057));
#18043=CARTESIAN_POINT('Ctrl Pts',(0.150485778196879,-0.000129396266831759,
0.822929130263837));
#18044=CARTESIAN_POINT('Ctrl Pts',(0.0816643079123276,0.126399869446589,
0.830871298386618));
#18045=CARTESIAN_POINT('Ctrl Pts',(-0.0619700581130299,0.137133869194964,
0.838813466509397));
#18046=CARTESIAN_POINT('Ctrl Pts',(-0.148833484480893,0.0222391564630926,
0.846755634632177));
#18047=CARTESIAN_POINT('Ctrl Pts',(-0.0993501488194509,-0.113028908304323,
0.854697802754957));
#18048=CARTESIAN_POINT('Ctrl Pts',(0.041148129789194,-0.144750881164039,
0.862639970877736));
#18049=CARTESIAN_POINT('Ctrl Pts',(0.143950494202948,-0.0438661760544617,
0.870582139000517));
#18050=CARTESIAN_POINT('Ctrl Pts',(0.114879417330645,0.0972044528644933,
0.878524307123298));
#18051=CARTESIAN_POINT('Ctrl Pts',(-0.0194330078274841,0.149225816766708,
0.886466475246077));
#18052=CARTESIAN_POINT('Ctrl Pts',(-0.135942801386891,0.0645410019599824,
0.894408643368857));
#18053=CARTESIAN_POINT('Ctrl Pts',(-0.127915022941288,-0.0792700011911429,
0.902350811491637));
#18054=CARTESIAN_POINT('Ctrl Pts',(-0.00270394227186439,-0.150461539534541,
0.910292979614417));
#18055=CARTESIAN_POINT('Ctrl Pts',(0.124984227305131,-0.0838148501630433,
0.918235147737197));
#18056=CARTESIAN_POINT('Ctrl Pts',(0.138174004553101,0.0596148525845174,
0.926177315859977));
#18057=CARTESIAN_POINT('Ctrl Pts',(0.0247821984756025,0.148431225898158,
0.934119483982757));
#18058=CARTESIAN_POINT('Ctrl Pts',(-0.11131264737753,0.101269347369872,
0.942061652105537));
#18059=CARTESIAN_POINT('Ctrl Pts',(-0.145433672650089,-0.0386656571445607,
0.950003820228317));
#18060=CARTESIAN_POINT('Ctrl Pts',(-0.0463225128062989,-0.143178947440692,
0.957945988351097));
#18061=CARTESIAN_POINT('Ctrl Pts',(0.0952248276606132,-0.116525612549003,
0.965888156473877));
#18062=CARTESIAN_POINT('Ctrl Pts',(0.149536443172165,0.0168771545685866,
0.973830324596656));
#18063=CARTESIAN_POINT('Ctrl Pts',(0.0668573142755158,0.134818714245386,
0.981772492719438));
#18064=CARTESIAN_POINT('Ctrl Pts',(-0.0770699830103684,0.129252481220654,
0.989714660842216));
#18065=CARTESIAN_POINT('Ctrl Pts',(-0.15039325815857,0.00527769678589187,
0.997656828964997));
#18066=CARTESIAN_POINT('Ctrl Pts',(-0.0859408583470751,-0.123532000103139,
1.00559899708778));
#18067=CARTESIAN_POINT('Ctrl Pts',(0.0572421967501742,-0.139173693973137,
1.01354116521056));
#18068=CARTESIAN_POINT('Ctrl Pts',(0.147985518909957,-0.0273179863069172,
1.02148333333334));
#18069=CARTESIAN_POINT('Ctrl Pts',(0.103158902618224,0.109563803299803,
1.02942550145612));
#18070=CARTESIAN_POINT('Ctrl Pts',(-0.0361718663885326,0.146073893166727,
1.0373676695789));
#18071=CARTESIAN_POINT('Ctrl Pts',(-0.142365489706367,0.0487652901517079,
1.04530983770168));
#18072=CARTESIAN_POINT('Ctrl Pts',(-0.118137698690712,-0.0932173284908804,
1.05325200582446));
#18073=CARTESIAN_POINT('Ctrl Pts',(0.0143163610725534,-0.149803297655807,
1.06119417394724));
#18074=CARTESIAN_POINT('Ctrl Pts',(0.133655163317704,-0.0691540562905145,
1.06913634207002));
#18075=CARTESIAN_POINT('Ctrl Pts',(0.130552105047211,0.0748474051030229,
1.0770785101928));
#18076=CARTESIAN_POINT('Ctrl Pts',(0.0078499064261323,0.150280954056111,
1.08502067831558));
#18077=CARTESIAN_POINT('Ctrl Pts',(-0.122043612932812,0.0880417101447944,
1.09296284643836));
#18078=CARTESIAN_POINT('Ctrl Pts',(-0.140132644828567,-0.0548527851276936,
1.10090501456114));
#18079=CARTESIAN_POINT('Ctrl Pts',(-0.0298457776877653,-0.147496493982489,
1.10884718268392));
#18080=CARTESIAN_POINT('Ctrl Pts',(0.107782887988268,-0.10501826145877,
1.1167893508067));
#18081=CARTESIAN_POINT('Ctrl Pts',(0.146671355310253,0.033667487497105,
1.12473151892948));
#18082=CARTESIAN_POINT('Ctrl Pts',(0.0511937930472066,0.141510359113225,
1.13267368705226));
#18083=CARTESIAN_POINT('Ctrl Pts',(-0.0911825429852659,0.119715203870077,
1.14061585517504));
#18084=CARTESIAN_POINT('Ctrl Pts',(-0.150026302104679,-0.0117513769282424,
1.14855802329782));
#18085=CARTESIAN_POINT('Ctrl Pts',(-0.0714305557085884,-0.132452489195471,
1.1565001914206));
#18086=CARTESIAN_POINT('Ctrl Pts',(0.0726029180563751,-0.131813513998426,
1.16444235954338));
#18087=CARTESIAN_POINT('Ctrl Pts',(0.150124660100533,-0.010419818262018,
1.17238452766616));
#18088=CARTESIAN_POINT('Ctrl Pts',(0.0901167906002831,0.120519501471002,
1.18032669578894));
#18089=CARTESIAN_POINT('Ctrl Pts',(-0.0524473171394798,0.141050576417769,
1.18826886391172));
#18090=CARTESIAN_POINT('Ctrl Pts',(-0.146964294261872,0.0323648326895764,
1.1962110320345));
#18091=CARTESIAN_POINT('Ctrl Pts',(-0.106846879624786,-0.105970422747861,
1.20415320015727));
#18092=CARTESIAN_POINT('Ctrl Pts',(0.0311532535456026,-0.14722588419309,
1.21209536828006));
#18093=CARTESIAN_POINT('Ctrl Pts',(0.140613805972886,-0.0536073106276968,
1.22003753640283));
#18094=CARTESIAN_POINT('Ctrl Pts',(0.121257666323848,0.0891210667609394,
1.22797970452562));
#18095=CARTESIAN_POINT('Ctrl Pts',(-0.00918295295119051,0.150205391241489,
1.2359218726484));
#18096=CARTESIAN_POINT('Ctrl Pts',(-0.131211043922368,0.0736861461587066,
1.24386404077118));
#18097=CARTESIAN_POINT('Ctrl Pts',(-0.133036338837895,-0.0703371788708997,
1.25180620889396));
#18098=CARTESIAN_POINT('Ctrl Pts',(-0.0129866800356469,-0.149924422041766,
1.25974837701674));
#18099=CARTESIAN_POINT('Ctrl Pts',(0.118960111851797,-0.0921654923014072,
1.26769054513952));
#18100=CARTESIAN_POINT('Ctrl Pts',(0.141927220045961,0.050026496908035,
1.2756327132623));
#18101=CARTESIAN_POINT('Ctrl Pts',(0.0348744139414821,0.146389075532006,
1.28357488138508));
#18102=CARTESIAN_POINT('Ctrl Pts',(-0.104126938119509,0.108644221848311,
1.29151704950786));
#18103=CARTESIAN_POINT('Ctrl Pts',(-0.147737317493493,-0.0286299004949125,
1.29945921763064));
#18104=CARTESIAN_POINT('Ctrl Pts',(-0.0560051364173496,-0.139676092720537,
1.30740138575342));
#18105=CARTESIAN_POINT('Ctrl Pts',(0.0870335032532438,-0.122764634549313,
1.3153435538762));
#18106=CARTESIAN_POINT('Ctrl Pts',(0.150340512633584,0.00661184096937889,
1.32328572199898));
#18107=CARTESIAN_POINT('Ctrl Pts',(0.0759201674095095,0.129931190880528,
1.33122789012176));
#18108=CARTESIAN_POINT('Ctrl Pts',(-0.0680508508044829,0.134220221643466,
1.33917005824454));
#18109=CARTESIAN_POINT('Ctrl Pts',(-0.149680298423566,0.0155497403439283,
1.34711222636732));
#18110=CARTESIAN_POINT('Ctrl Pts',(-0.0941872156892785,-0.117365900463673,
1.3550543944901));
#18111=CARTESIAN_POINT('Ctrl Pts',(0.0475910332998192,-0.142762319241037,
1.36299656261288));
#18112=CARTESIAN_POINT('Ctrl Pts',(0.145771005694385,-0.0373737865856905,
1.37093873073566));
#18113=CARTESIAN_POINT('Ctrl Pts',(0.110409762917901,0.10225297323032,1.37888089885844));
#18114=CARTESIAN_POINT('Ctrl Pts',(-0.0260981686868614,0.148205506441964,
1.38682306698121));
#18115=CARTESIAN_POINT('Ctrl Pts',(-0.138697490589939,0.0583865667538053,
1.394765235104));
#18116=CARTESIAN_POINT('Ctrl Pts',(-0.124235673603468,-0.0849204601545819,
1.40270740322677));
#18117=CARTESIAN_POINT('Ctrl Pts',(0.0040388053119065,-0.150431633134115,
1.41064957134956));
#18118=CARTESIAN_POINT('Ctrl Pts',(0.12861328245382,-0.0781319533624403,
1.41859173947234));
#18119=CARTESIAN_POINT('Ctrl Pts',(0.1353648581188,0.0657445800149866,1.42653390759512));
#18120=CARTESIAN_POINT('Ctrl Pts',(0.0181081687242482,0.149392404544468,
1.43447607571789));
#18121=CARTESIAN_POINT('Ctrl Pts',(-0.115737181672069,0.0961812857364522,
1.44241824384068));
#18122=CARTESIAN_POINT('Ctrl Pts',(-0.143555918690644,-0.0451414811888502,
1.45036041196346));
#18123=CARTESIAN_POINT('Ctrl Pts',(-0.0398616700558823,-0.145110565703753,
1.45830258008624));
#18124=CARTESIAN_POINT('Ctrl Pts',(0.100348034367198,-0.112142416378873,
1.46624474820902));
#18125=CARTESIAN_POINT('Ctrl Pts',(0.14863229283285,0.0235577176564554,
1.4741869163318));
#18126=CARTESIAN_POINT('Ctrl Pts',(0.0607471474677608,0.137680339497592,
1.48212908445458));
#18127=CARTESIAN_POINT('Ctrl Pts',(-0.0827754224726193,0.125666453945577,
1.49007125257736));
#18128=CARTESIAN_POINT('Ctrl Pts',(-0.150492272191201,-0.00145719475437189,
1.49801342070014));
#18129=CARTESIAN_POINT('Ctrl Pts',(-0.0802951178786721,-0.12727177793954,
1.50595558882292));
#18130=CARTESIAN_POINT('Ctrl Pts',(0.0633700050447994,-0.136443062004882,
1.5138977569457));
#18131=CARTESIAN_POINT('Ctrl Pts',(0.149155357006591,-0.0207133070603065,
1.52183992506848));
#18132=CARTESIAN_POINT('Ctrl Pts',(0.0979555318420461,0.114182655252422,
1.52978209319126));
#18133=CARTESIAN_POINT('Ctrl Pts',(0.00450803278943675,0.134083974545181,
1.53507687193978));
#18134=CARTESIAN_POINT('Ctrl Pts',(-0.0361033354337414,0.122073089461022,
1.53772426131404));
#18135=CARTESIAN_POINT('Ctrl Pts',(-0.0592743564846203,0.123319225136773,
-0.00549926131403157));
#18136=CARTESIAN_POINT('Ctrl Pts',(-0.100300290071938,0.10359978715075,
-0.00285187193977157));
#18137=CARTESIAN_POINT('Ctrl Pts',(-0.160414584165772,0.0203416160441626,
0.00244290680874841));
#18138=CARTESIAN_POINT('Ctrl Pts',(-0.103922107946056,-0.124084444561314,
0.0103850749315284));
#18139=CARTESIAN_POINT('Ctrl Pts',(0.0479099321398382,-0.154436663180837,
0.0183272430543084));
#18140=CARTESIAN_POINT('Ctrl Pts',(0.155781551077148,-0.0435098515708298,
0.0262694111770884));
#18141=CARTESIAN_POINT('Ctrl Pts',(0.120977930992648,0.107381072623318,
0.0342115792998684));
#18142=CARTESIAN_POINT('Ctrl Pts',(-0.0246731903087699,0.159844935900913,
0.0421537474226484));
#18143=CARTESIAN_POINT('Ctrl Pts',(-0.147710978397823,0.0659033513787588,
0.0500959155454284));
#18144=CARTESIAN_POINT('Ctrl Pts',(-0.135435684249567,-0.0884277117007276,
0.0580380836682085));
#18145=CARTESIAN_POINT('Ctrl Pts',(0.000915427738408385,-0.16174188059703,
0.0659802517909884));
#18146=CARTESIAN_POINT('Ctrl Pts',(0.13642643003965,-0.0868880976295618,
0.0739224199137684));
#18147=CARTESIAN_POINT('Ctrl Pts',(0.146957588340267,0.0675663355536457,
0.0818645880365484));
#18148=CARTESIAN_POINT('Ctrl Pts',(0.0228600865593111,0.160121891352391,
0.0898067561593285));
#18149=CARTESIAN_POINT('Ctrl Pts',(-0.122179386207322,0.105989962368389,
0.0977489242821083));
#18150=CARTESIAN_POINT('Ctrl Pts',(-0.155290103436038,-0.0452399862206161,
0.105691092404888));
#18151=CARTESIAN_POINT('Ctrl Pts',(-0.0461390722131997,-0.155025288408554,
0.113633260527668));
#18152=CARTESIAN_POINT('Ctrl Pts',(0.105280057525145,-0.122791590307548,
0.121575428650448));
#18153=CARTESIAN_POINT('Ctrl Pts',(0.160251855424436,0.0219318669073289,
0.129517596773229));
#18154=CARTESIAN_POINT('Ctrl Pts',(0.0684164816681947,0.146563455853242,
0.137459764896008));
#18155=CARTESIAN_POINT('Ctrl Pts',(-0.086095413359615,0.136927875387926,
0.145401933018789));
#18156=CARTESIAN_POINT('Ctrl Pts',(-0.16173506727009,0.00185228698694943,
0.153344101141568));
#18157=CARTESIAN_POINT('Ctrl Pts',(-0.0892087826023274,-0.134920182928699,
0.161286269264348));
#18158=CARTESIAN_POINT('Ctrl Pts',(0.0650419110192955,-0.148091906331324,
0.169228437387128));
#18159=CARTESIAN_POINT('Ctrl Pts',(0.159707532494063,-0.025596228460074,
0.177170605509908));
#18160=CARTESIAN_POINT('Ctrl Pts',(0.108064646638443,0.120348223746572,
0.185112773632688));
#18161=CARTESIAN_POINT('Ctrl Pts',(-0.0425765573421325,0.156041339440091,
0.193054941755468));
#18162=CARTESIAN_POINT('Ctrl Pts',(-0.154213260793436,0.0487845573223287,
0.200997109878248));
#18163=CARTESIAN_POINT('Ctrl Pts',(-0.124574774400312,-0.103163891052585,
0.208939278001028));
#18164=CARTESIAN_POINT('Ctrl Pts',(0.0191870033818907,-0.160603616835255,
0.216881446123808));
#18165=CARTESIAN_POINT('Ctrl Pts',(0.145371514918136,-0.0709139301387177,
0.224823614246588));
#18166=CARTESIAN_POINT('Ctrl Pts',(0.138380784202201,0.0837402018183176,
0.232765782369368));
#18167=CARTESIAN_POINT('Ctrl Pts',(0.00461903876105218,0.161679705957985,
0.240707950492149));
#18168=CARTESIAN_POINT('Ctrl Pts',(-0.133374220718213,0.0915039894496894,
0.248650118614928));
#18169=CARTESIAN_POINT('Ctrl Pts',(-0.149182991964712,-0.0624987819548612,
0.256592286737709));
#18170=CARTESIAN_POINT('Ctrl Pts',(-0.0283248164207669,-0.159246248345813,
0.264534454860488));
#18171=CARTESIAN_POINT('Ctrl Pts',(0.118481800883715,-0.110107791262854,
0.272476622983269));
#18172=CARTESIAN_POINT('Ctrl Pts',(0.156746916480749,0.0399007144198201,
0.280418791106048));
#18173=CARTESIAN_POINT('Ctrl Pts',(0.0514157533588968,0.153356066537929,
0.288360959228829));
#18174=CARTESIAN_POINT('Ctrl Pts',(-0.101017521980764,0.126321506839912,
0.296303127351608));
#18175=CARTESIAN_POINT('Ctrl Pts',(-0.160908369261695,-0.0164365306249019,
0.304245295474388));
#18176=CARTESIAN_POINT('Ctrl Pts',(-0.0733906195540655,-0.144137017448375,
0.312187463597168));
#18177=CARTESIAN_POINT('Ctrl Pts',(0.0813604773699057,-0.13979318853071,
0.320129631719948));
#18178=CARTESIAN_POINT('Ctrl Pts',(0.161577018543625,-0.00738443741900211,
0.328071799842729));
#18179=CARTESIAN_POINT('Ctrl Pts',(0.0937724112935796,0.131789217000595,
0.336013967965508));
#18180=CARTESIAN_POINT('Ctrl Pts',(-0.0599373583072218,0.150230409426965,
0.343956136088289));
#18181=CARTESIAN_POINT('Ctrl Pts',(-0.158738350099833,0.0310451130618767,
0.351898304211068));
#18182=CARTESIAN_POINT('Ctrl Pts',(-0.112118705390683,-0.116580696253536,
0.359840472333849));
#18183=CARTESIAN_POINT('Ctrl Pts',(0.0372131918485748,-0.15740661101073,
0.367782640456628));
#18184=CARTESIAN_POINT('Ctrl Pts',(0.152453982298084,-0.0540318990865351,
0.375724808579408));
#18185=CARTESIAN_POINT('Ctrl Pts',(0.128031262769868,0.0988415833088236,
0.383666976702188));
#18186=CARTESIAN_POINT('Ctrl Pts',(-0.0136812466069205,0.161166021011634,
0.391609144824968));
#18187=CARTESIAN_POINT('Ctrl Pts',(-0.142860328563903,0.0758458262533652,
0.399551312947749));
#18188=CARTESIAN_POINT('Ctrl Pts',(-0.141164672957165,-0.0789569372907697,
0.407493481070528));
#18189=CARTESIAN_POINT('Ctrl Pts',(-0.0101476745237983,-0.161427034722196,
0.415435649193308));
#18190=CARTESIAN_POINT('Ctrl Pts',(0.130165636283581,-0.0960133843187101,
0.423377817316089));
#18191=CARTESIAN_POINT('Ctrl Pts',(0.151233851831306,0.0573583899504574,
0.431319985438868));
#18192=CARTESIAN_POINT('Ctrl Pts',(0.0337563222576384,0.158183986373718,
0.439262153561649));
#18193=CARTESIAN_POINT('Ctrl Pts',(-0.114645466422773,0.114096800420287,
0.447204321684428));
#18194=CARTESIAN_POINT('Ctrl Pts',(-0.158020229883659,-0.0345147763277912,
0.455146489807208));
#18195=CARTESIAN_POINT('Ctrl Pts',(-0.0566322287360923,-0.151507272121918,
0.463088657929988));
#18196=CARTESIAN_POINT('Ctrl Pts',(0.0966367119836487,-0.129703541718919,
0.471030826052768));
#18197=CARTESIAN_POINT('Ctrl Pts',(0.161376496659739,0.0109219578497271,
0.478972994175549));
#18198=CARTESIAN_POINT('Ctrl Pts',(0.0782788315581001,0.141541821972661,
0.486915162298328));
#18199=CARTESIAN_POINT('Ctrl Pts',(-0.0765302851406724,0.142494836024782,
0.494857330421108));
#18200=CARTESIAN_POINT('Ctrl Pts',(-0.161229798395673,0.0129079412274925,
0.502799498543889));
#18201=CARTESIAN_POINT('Ctrl Pts',(-0.0982262525537151,-0.128503953817366,
0.510741666666668));
#18202=CARTESIAN_POINT('Ctrl Pts',(0.0547626317937811,-0.152193025452748,
0.518683834789449));
#18203=CARTESIAN_POINT('Ctrl Pts',(0.157583319439253,-0.0364576503898468,
0.526626002912228));
#18204=CARTESIAN_POINT('Ctrl Pts',(0.116041497328862,0.112676677866884,
0.534568171035008));
#18205=CARTESIAN_POINT('Ctrl Pts',(-0.0318062577307366,0.158587593482618,
0.542510339157789));
#18206=CARTESIAN_POINT('Ctrl Pts',(-0.150516213127973,0.0592159811457737,
0.550452507280567));
#18207=CARTESIAN_POINT('Ctrl Pts',(-0.131337854181896,-0.0944035534094825,
0.558394675403349));
#18208=CARTESIAN_POINT('Ctrl Pts',(0.00815947204521347,-0.161539734596121,
0.566336843526128));
#18209=CARTESIAN_POINT('Ctrl Pts',(0.140181883624494,-0.080688923285235,
0.574279011648909));
#18210=CARTESIAN_POINT('Ctrl Pts',(0.143783288371658,0.0740812312429708,
0.582221179771688));
#18211=CARTESIAN_POINT('Ctrl Pts',(0.0156644295519346,0.160985367298567,
0.590163347894469));
#18212=CARTESIAN_POINT('Ctrl Pts',(-0.126804656005353,0.100410368253513,
0.598105516017247));
#18213=CARTESIAN_POINT('Ctrl Pts',(-0.153107649524464,-0.0521508436608248,
0.606047684140029));
#18214=CARTESIAN_POINT('Ctrl Pts',(-0.0391483067326994,-0.156936525122116,
0.613989852262808));
#18215=CARTESIAN_POINT('Ctrl Pts',(0.110674906884577,-0.117952226869747,
0.621932020385589));
#18216=CARTESIAN_POINT('Ctrl Pts',(0.159108535730396,0.0290884288879846,
0.629874188508368));
#18217=CARTESIAN_POINT('Ctrl Pts',(0.061782400006242,0.14948109541648,0.637816356631148));
#18218=CARTESIAN_POINT('Ctrl Pts',(-0.0921427612707386,0.132933721767072,
0.645758524753929));
#18219=CARTESIAN_POINT('Ctrl Pts',(-0.161655687038194,-0.0053945978210935,
0.653700692876707));
#18220=CARTESIAN_POINT('Ctrl Pts',(-0.0830753959589387,-0.138780911597048,
0.661642860999489));
#18221=CARTESIAN_POINT('Ctrl Pts',(0.0716104924784035,-0.145029652845349,
0.669585029122267));
#18222=CARTESIAN_POINT('Ctrl Pts',(0.160693812980115,-0.0184163326249747,
0.677527197245049));
#18223=CARTESIAN_POINT('Ctrl Pts',(0.102565092089392,0.125068240261613,
0.685469365367828));
#18224=CARTESIAN_POINT('Ctrl Pts',(-0.0495237900674707,0.153977456320057,
0.693411533490608));
#18225=CARTESIAN_POINT('Ctrl Pts',(-0.156243792750268,0.0418275036842162,
0.701353701613389));
#18226=CARTESIAN_POINT('Ctrl Pts',(-0.119828429739121,-0.108640739429086,
0.709295869736167));
#18227=CARTESIAN_POINT('Ctrl Pts',(0.0263620853553792,-0.159582904138124,
0.717238037858949));
#18228=CARTESIAN_POINT('Ctrl Pts',(0.148402221984423,-0.0643307340819919,
0.725180205981728));
#18229=CARTESIAN_POINT('Ctrl Pts',(0.134490677336207,0.0898549973406614,
0.733122374104509));
#18230=CARTESIAN_POINT('Ctrl Pts',(-0.00262814450422035,0.161724320044658,
0.741064542227287));
#18231=CARTESIAN_POINT('Ctrl Pts',(-0.137339315979238,0.0854375510170853,
0.749006710350069));
#18232=CARTESIAN_POINT('Ctrl Pts',(-0.146233564613262,-0.0691187920752458,
0.756948878472847));
#18233=CARTESIAN_POINT('Ctrl Pts',(-0.0211628449166461,-0.160355220783347,
0.764891046595629));
#18234=CARTESIAN_POINT('Ctrl Pts',(0.12329521486528,-0.104689793336152,
0.772833214718408));
#18235=CARTESIAN_POINT('Ctrl Pts',(0.154802191231926,0.0468822399980663,
0.780775382841188));
#18236=CARTESIAN_POINT('Ctrl Pts',(0.0444944569967772,0.155505325098544,
0.788717550963968));
#18237=CARTESIAN_POINT('Ctrl Pts',(-0.106574770936664,0.121669556739719,
0.796659719086747));
#18238=CARTESIAN_POINT('Ctrl Pts',(-0.160010559849905,-0.0236280251811701,
0.804601887209529));
#18239=CARTESIAN_POINT('Ctrl Pts',(-0.0668602374312443,-0.147279908636853,
0.812544055332307));
#18240=CARTESIAN_POINT('Ctrl Pts',(0.0875409312876049,-0.13600826514128,
0.820486223455089));
#18241=CARTESIAN_POINT('Ctrl Pts',(0.161745613525436,-0.000139078116330951,
0.828428391577867));
#18242=CARTESIAN_POINT('Ctrl Pts',(0.0877746970157421,0.135857518751215,
0.836370559700649));
#18243=CARTESIAN_POINT('Ctrl Pts',(-0.0666068593976089,0.147394671269449,
0.844312727823428));
#18244=CARTESIAN_POINT('Ctrl Pts',(-0.159969689820096,0.0239031624749592,
0.852254895946208));
#18245=CARTESIAN_POINT('Ctrl Pts',(-0.106783850056725,-0.121486098811777,
0.860197064068988));
#18246=CARTESIAN_POINT('Ctrl Pts',(0.0442269666803361,-0.155581612845794,
0.868139232191768));
#18247=CARTESIAN_POINT('Ctrl Pts',(0.154721338329289,-0.0471483860066884,
0.876081400314548));
#18248=CARTESIAN_POINT('Ctrl Pts',(0.123475068941597,0.104477606152275,
0.884023568437328));
#18249=CARTESIAN_POINT('Ctrl Pts',(-0.0208870486723946,0.160391377683462,
0.891965736560109));
#18250=CARTESIAN_POINT('Ctrl Pts',(-0.146114483894434,0.0693701696243073,
0.899907904682887));
#18251=CARTESIAN_POINT('Ctrl Pts',(-0.137486040957907,-0.0852012404790134,
0.907850072805669));
#18252=CARTESIAN_POINT('Ctrl Pts',(-0.00290626002629624,-0.161719561247554,
0.915792240928448));
#18253=CARTESIAN_POINT('Ctrl Pts',(0.134335953660838,-0.0900861498315643,
0.923734409051229));
#18254=CARTESIAN_POINT('Ctrl Pts',(0.148512632937768,0.0640754297319473,
0.931676577174007));
#18255=CARTESIAN_POINT('Ctrl Pts',(0.0266364831612253,0.159537332941991,
0.939618745296788));
#18256=CARTESIAN_POINT('Ctrl Pts',(-0.119641421660886,0.10884664928423,
0.947560913419568));
#18257=CARTESIAN_POINT('Ctrl Pts',(-0.156315493011378,-0.0415587473590326,
0.955503081542348));
#18258=CARTESIAN_POINT('Ctrl Pts',(-0.0497885138626987,-0.153892061929087,
0.963445249665127));
#18259=CARTESIAN_POINT('Ctrl Pts',(0.102349858952582,-0.125244437839883,
0.971387417787908));
#18260=CARTESIAN_POINT('Ctrl Pts',(0.160725246166783,0.018139958160622,
0.979329585910688));
#18261=CARTESIAN_POINT('Ctrl Pts',(0.0718597959603077,0.14490628889729,
0.987271754033468));
#18262=CARTESIAN_POINT('Ctrl Pts',(-0.0828366097831417,0.138923572215364,
0.995213922156248));
#18263=CARTESIAN_POINT('Ctrl Pts',(-0.161646170836971,0.00567259122332548,
1.00315609027903));
#18264=CARTESIAN_POINT('Ctrl Pts',(-0.0923712328620446,-0.132775066096718,
1.01109825840181));
#18265=CARTESIAN_POINT('Ctrl Pts',(0.0615252440718216,-0.149587122371362,
1.01904042652459));
#18266=CARTESIAN_POINT('Ctrl Pts',(0.159058276707423,-0.0293620068848675,
1.02698259464737));
#18267=CARTESIAN_POINT('Ctrl Pts',(0.1108775872014,0.117761723381742,1.03492476277015));
#18268=CARTESIAN_POINT('Ctrl Pts',(-0.0388783630684312,0.157003616909169,
1.04286693089293));
#18269=CARTESIAN_POINT('Ctrl Pts',(-0.153017738641585,0.0524140677533946,
1.05080909901571));
#18270=CARTESIAN_POINT('Ctrl Pts',(-0.126977145509477,-0.10019215216626,
1.05875126713849));
#18271=CARTESIAN_POINT('Ctrl Pts',(0.0153875577671049,-0.161012067570745,
1.06669343526127));
#18272=CARTESIAN_POINT('Ctrl Pts',(0.143655677305146,-0.0743283876822416,
1.07463560338405));
#18273=CARTESIAN_POINT('Ctrl Pts',(0.140320438123209,0.080447731368589,
1.08257777150683));
#18274=CARTESIAN_POINT('Ctrl Pts',(0.00843726195408678,0.161525463776335,
1.09051993962961));
#18275=CARTESIAN_POINT('Ctrl Pts',(-0.131175312957834,0.094629277223576,
1.09846210775239));
#18276=CARTESIAN_POINT('Ctrl Pts',(-0.150617825048456,-0.0589570489009974,
1.10640427587517));
#18277=CARTESIAN_POINT('Ctrl Pts',(-0.0320789358376135,-0.158532661344495,
1.11434644399795));
#18278=CARTESIAN_POINT('Ctrl Pts',(0.115847554194776,-0.112876069317329,
1.12228861212073));
#18279=CARTESIAN_POINT('Ctrl Pts',(0.157645783113317,0.0361865984037055,
1.13023078024351));
#18280=CARTESIAN_POINT('Ctrl Pts',(0.0550242791334153,0.152098624396442,
1.13817294836629));
#18281=CARTESIAN_POINT('Ctrl Pts',(-0.0980051173916675,0.128672684756662,
1.14611511648907));
#18282=CARTESIAN_POINT('Ctrl Pts',(-0.161251757937727,-0.0126306531673768,
1.15405728461185));
#18283=CARTESIAN_POINT('Ctrl Pts',(-0.0767752221903169,-0.142363015193798,
1.16199945273463));
#18284=CARTESIAN_POINT('Ctrl Pts',(0.0780353045016797,-0.141676229794458,
1.16994162085741));
#18285=CARTESIAN_POINT('Ctrl Pts',(0.161357475398708,-0.0111994629512984,
1.17788378898019));
#18286=CARTESIAN_POINT('Ctrl Pts',(0.0968596219472387,0.129537162519796,
1.18582595710297));
#18287=CARTESIAN_POINT('Ctrl Pts',(-0.0563715959749383,0.151604439264423,
1.19376812522575));
#18288=CARTESIAN_POINT('Ctrl Pts',(-0.157960640709981,0.0347864747270306,
1.20171029334853));
#18289=CARTESIAN_POINT('Ctrl Pts',(-0.114841510641486,-0.113899474410655,
1.20965246147131));
#18290=CARTESIAN_POINT('Ctrl Pts',(0.03348424129126,-0.158241803650584,
1.21759462959409));
#18291=CARTESIAN_POINT('Ctrl Pts',(0.151134988234409,-0.0576183839484237,
1.22553679771687));
#18292=CARTESIAN_POINT('Ctrl Pts',(0.130330559267559,0.0957893948119858,
1.23347896583965));
#18293=CARTESIAN_POINT('Ctrl Pts',(-0.0098700513554357,0.16144424710618,
1.24142113396243));
#18294=CARTESIAN_POINT('Ctrl Pts',(-0.141028680947982,0.0791995832534545,
1.24936330208521));
#18295=CARTESIAN_POINT('Ctrl Pts',(-0.142990550365238,-0.0756000353418,
1.25730547020799));
#18296=CARTESIAN_POINT('Ctrl Pts',(-0.013958385670676,-0.161142254877177,
1.26524763833077));
#18297=CARTESIAN_POINT('Ctrl Pts',(0.127861094297897,-0.0990616141723472,
1.27318980645355));
#18298=CARTESIAN_POINT('Ctrl Pts',(0.152546676219863,0.0537696421008814,
1.28113197457633));
#18299=CARTESIAN_POINT('Ctrl Pts',(0.0374838310097642,0.157342382244044,
1.28907414269911));
#18300=CARTESIAN_POINT('Ctrl Pts',(-0.111918054267102,0.116773335855419,
1.29701631082189));
#18301=CARTESIAN_POINT('Ctrl Pts',(-0.158791504053787,-0.0307720827589687,
1.30495847894467));
#18302=CARTESIAN_POINT('Ctrl Pts',(-0.060195622861772,-0.150127112226926,
1.31290064706745));
#18303=CARTESIAN_POINT('Ctrl Pts',(0.0935456330135535,-0.131950283756556,
1.32084281519023));
#18304=CARTESIAN_POINT('Ctrl Pts',(0.161589478720268,0.00710656041347678,
1.32878498331301));
#18305=CARTESIAN_POINT('Ctrl Pts',(0.0816007612396376,0.139653065139265,
1.33672715143579));
#18306=CARTESIAN_POINT('Ctrl Pts',(-0.0731426367739486,0.144263015132499,
1.34466931955857));
#18307=CARTESIAN_POINT('Ctrl Pts',(-0.160879865135934,0.0167132224867059,
1.35261148768135));
#18308=CARTESIAN_POINT('Ctrl Pts',(-0.101234609479067,-0.126147598829082,
1.36055365580413));
#18309=CARTESIAN_POINT('Ctrl Pts',(0.051151949184981,-0.153444260252591,
1.36849582392691));
#18310=CARTESIAN_POINT('Ctrl Pts',(0.15667806641111,-0.0401702148435725,
1.37643799204969));
#18311=CARTESIAN_POINT('Ctrl Pts',(0.118670980449659,0.10990387323047,1.38438016017247));
#18312=CARTESIAN_POINT('Ctrl Pts',(-0.0280509185434417,0.159294724422008,
1.39232232829525));
#18313=CARTESIAN_POINT('Ctrl Pts',(-0.149075287902345,0.0627552395607943,
1.40026449641803));
#18314=CARTESIAN_POINT('Ctrl Pts',(-0.133531390736797,-0.0912744851582948,
1.40820666454081));
#18315=CARTESIAN_POINT('Ctrl Pts',(0.00434100186018791,-0.161687417152987,
1.41614883266359));
#18316=CARTESIAN_POINT('Ctrl Pts',(0.138236546518021,-0.0839780402106489,
1.42409100078637));
#18317=CARTESIAN_POINT('Ctrl Pts',(0.145493297031458,0.07066380330362,1.43203316890915));
#18318=CARTESIAN_POINT('Ctrl Pts',(0.0194630807988606,0.160570430100525,
1.43997533703193));
#18319=CARTESIAN_POINT('Ctrl Pts',(-0.124397014000637,0.103377882332206,
1.44791750515471));
#18320=CARTESIAN_POINT('Ctrl Pts',(-0.15429723939393,-0.0485191136187331,
1.45585967327749));
#18321=CARTESIAN_POINT('Ctrl Pts',(-0.042844249846,-0.155968210152522,1.46380184140027));
#18322=CARTESIAN_POINT('Ctrl Pts',(0.107856400646442,-0.120533276677448,
1.47174400952305));
#18323=CARTESIAN_POINT('Ctrl Pts',(0.159753444358638,0.0253203827049868,
1.47968617764583));
#18324=CARTESIAN_POINT('Ctrl Pts',(0.0652924466007548,0.147982030257331,
1.48762834576861));
#18325=CARTESIAN_POINT('Ctrl Pts',(-0.0889689487809616,0.13506922671723,
1.49557051389139));
#18326=CARTESIAN_POINT('Ctrl Pts',(-0.161752593421533,-0.00156622680492735,
1.50351268201417));
#18327=CARTESIAN_POINT('Ctrl Pts',(-0.086303059730943,-0.136794666273195,
1.51145485013695));
#18328=CARTESIAN_POINT('Ctrl Pts',(0.0681115549116652,-0.14665217563879,
1.51939701825973));
#18329=CARTESIAN_POINT('Ctrl Pts',(0.160315645894948,-0.02226314405755,
1.52733918638251));
#18330=CARTESIAN_POINT('Ctrl Pts',(0.105284883301553,0.122726172858702,
1.53528135450529));
#18331=CARTESIAN_POINT('Ctrl Pts',(0.00484533846358528,0.144116573583224,
1.54057613325381));
#18332=CARTESIAN_POINT('Ctrl Pts',(-0.0388047044047284,0.131206995015745,
1.54322352262807));
#18333=CARTESIAN_POINT('Ctrl Pts',(-0.0634007094575145,0.131904027763688,
-3.88578058618805E-16));
#18334=CARTESIAN_POINT('Ctrl Pts',(-0.107282641710421,0.110811831533068,
0.00264738937425961));
#18335=CARTESIAN_POINT('Ctrl Pts',(-0.171581760589518,0.0217576868851663,
0.0079421681227796));
#18336=CARTESIAN_POINT('Ctrl Pts',(-0.111156590520044,-0.1327225175337,
0.0158843362455596));
#18337=CARTESIAN_POINT('Ctrl Pts',(0.0512451567233008,-0.165187689797298,
0.0238265043683396));
#18338=CARTESIAN_POINT('Ctrl Pts',(0.16662620135312,-0.0465387668729445,
0.0317686724911196));
#18339=CARTESIAN_POINT('Ctrl Pts',(0.129399745666171,0.114856349193662,
0.0397108406138996));
#18340=CARTESIAN_POINT('Ctrl Pts',(-0.026390801400978,0.170972456562021,
0.0476530087366796));
#18341=CARTESIAN_POINT('Ctrl Pts',(-0.157993800025737,0.070491178324729,
0.0555951768594596));
#18342=CARTESIAN_POINT('Ctrl Pts',(-0.144863967768493,-0.0945835600760224,
0.0635373449822396));
#18343=CARTESIAN_POINT('Ctrl Pts',(0.000979154756195248,-0.17300145605975,
0.0714795131050195));
#18344=CARTESIAN_POINT('Ctrl Pts',(0.145923683802689,-0.0929367665856833,
0.0794216812277997));
#18345=CARTESIAN_POINT('Ctrl Pts',(0.157187963117837,0.0722699302633024,
0.0873638493505794));
#18346=CARTESIAN_POINT('Ctrl Pts',(0.0244514793930555,0.171268692120756,
0.0953060174733598));
#18347=CARTESIAN_POINT('Ctrl Pts',(-0.130684839550095,0.113368397534175,
0.103248185596139));
#18348=CARTESIAN_POINT('Ctrl Pts',(-0.166100541844429,-0.0483893439312075,
0.11119035371892));
#18349=CARTESIAN_POINT('Ctrl Pts',(-0.0493510193195793,-0.165817291858885,
0.119132521841699));
#18350=CARTESIAN_POINT('Ctrl Pts',(0.112609073040783,-0.131339661914923,
0.12707468996448));
#18351=CARTESIAN_POINT('Ctrl Pts',(0.17140770357293,0.0234586422209967,
0.135016858087259));
#18352=CARTESIAN_POINT('Ctrl Pts',(0.0731792588499177,0.156766393306209,
0.14295902621004));
#18353=CARTESIAN_POINT('Ctrl Pts',(-0.0920889000195865,0.146460037003638,
0.150901194332819));
#18354=CARTESIAN_POINT('Ctrl Pts',(-0.172994168426659,0.00198123296575728,
0.1588433624556));
#18355=CARTESIAN_POINT('Ctrl Pts',(-0.0954190048152776,-0.144312580095855,
0.16678553057838));
#18356=CARTESIAN_POINT('Ctrl Pts',(0.0695697692503139,-0.158401246055831,
0.17472769870116));
#18357=CARTESIAN_POINT('Ctrl Pts',(0.170825487889685,-0.0273780963649298,
0.18266986682394));
#18358=CARTESIAN_POINT('Ctrl Pts',(0.115587509852263,0.128726201683253,
0.19061203494672));
#18359=CARTESIAN_POINT('Ctrl Pts',(-0.0455405018601966,0.16690407474553,
0.198554203069499));
#18360=CARTESIAN_POINT('Ctrl Pts',(-0.164948735370872,0.0521806684752238,
0.20649637119228));
#18361=CARTESIAN_POINT('Ctrl Pts',(-0.133246981425072,-0.110345590758605,
0.214438539315059));
#18362=CARTESIAN_POINT('Ctrl Pts',(0.0205226964731592,-0.171783952668295,
0.22238070743784));
#18363=CARTESIAN_POINT('Ctrl Pts',(0.155491476033395,-0.0758505658746651,
0.230322875560619));
#18364=CARTESIAN_POINT('Ctrl Pts',(0.148014089296488,0.0895697316726553,
0.2382650436834));
#18365=CARTESIAN_POINT('Ctrl Pts',(0.00494059070111224,0.172934953166096,
0.24620721180618));
#18366=CARTESIAN_POINT('Ctrl Pts',(-0.142658996543838,0.0978739912732451,
0.25414937992896));
#18367=CARTESIAN_POINT('Ctrl Pts',(-0.159568287038446,-0.0668496016012732,
0.262091548051739));
#18368=CARTESIAN_POINT('Ctrl Pts',(-0.0302966335331915,-0.170332091689456,
0.27003371617452));
#18369=CARTESIAN_POINT('Ctrl Pts',(0.126729848780061,-0.11777288690896,
0.2779758842973));
#18370=CARTESIAN_POINT('Ctrl Pts',(0.167658770158652,0.0426783815482623,
0.28591805242008));
#18371=CARTESIAN_POINT('Ctrl Pts',(0.0549950338320791,0.164031867990689,
0.293860220542859));
#18372=CARTESIAN_POINT('Ctrl Pts',(-0.108049803339193,0.135115311719503,
0.30180238866564));
#18373=CARTESIAN_POINT('Ctrl Pts',(-0.1721099202737,-0.0175807510100837,
0.309744556788419));
#18374=CARTESIAN_POINT('Ctrl Pts',(-0.0784996687135917,-0.154171039675278,
0.3176867249112));
#18375=CARTESIAN_POINT('Ctrl Pts',(0.087024343965547,-0.14952481740522,
0.325628893033979));
#18376=CARTESIAN_POINT('Ctrl Pts',(0.172825117221703,-0.00789850112384905,
0.33357106115676));
#18377=CARTESIAN_POINT('Ctrl Pts',(0.100300328103893,0.140963653630822,
0.341513229279539));
#18378=CARTESIAN_POINT('Ctrl Pts',(-0.0641098658012952,0.160688619913292,
0.349455397402319));
#18379=CARTESIAN_POINT('Ctrl Pts',(-0.16978883637574,0.033206302186043,
0.357397565525099));
#18380=CARTESIAN_POINT('Ctrl Pts',(-0.119923789760104,-0.124696399756661,
0.36533973364788));
#18381=CARTESIAN_POINT('Ctrl Pts',(0.0398037685148125,-0.168364388974385,
0.373281901770659));
#18382=CARTESIAN_POINT('Ctrl Pts',(0.163066985633654,-0.0577933011607096,
0.38122406989344));
#18383=CARTESIAN_POINT('Ctrl Pts',(0.136944091404129,0.10572238784759,0.38916623801622));
#18384=CARTESIAN_POINT('Ctrl Pts',(-0.0146336593526265,0.172385508313924,
0.397108406138999));
#18385=CARTESIAN_POINT('Ctrl Pts',(-0.152805474769431,0.0811257933285562,
0.40505057426178));
#18386=CARTESIAN_POINT('Ctrl Pts',(-0.150991776994562,-0.0844534827151793,
0.412992742384559));
#18387=CARTESIAN_POINT('Ctrl Pts',(-0.0108540995180527,-0.172664692355881,
0.42093491050734));
#18388=CARTESIAN_POINT('Ctrl Pts',(0.139227048201004,-0.102697305280782,
0.428877078630119));
#18389=CARTESIAN_POINT('Ctrl Pts',(0.16176191642983,0.0613513639265466,
0.4368192467529));
#18390=CARTESIAN_POINT('Ctrl Pts',(0.0361062507758455,0.169195880912067,
0.444761414875679));
#18391=CARTESIAN_POINT('Ctrl Pts',(-0.12262644992489,0.12203958882886,0.45270358299846));
#18392=CARTESIAN_POINT('Ctrl Pts',(-0.169020724600573,-0.0369175042249048,
0.460645751121239));
#18393=CARTESIAN_POINT('Ctrl Pts',(-0.0605746513833496,-0.162054370729346,
0.468587919244019));
#18394=CARTESIAN_POINT('Ctrl Pts',(0.103364025571403,-0.138732785167649,
0.4765300873668));
#18395=CARTESIAN_POINT('Ctrl Pts',(0.172610636112938,0.0116822841681558,
0.484472255489579));
#18396=CARTESIAN_POINT('Ctrl Pts',(0.083728171010617,0.151395181039277,
0.49241442361236));
#18397=CARTESIAN_POINT('Ctrl Pts',(-0.081857900459256,0.152414538660527,
0.500356591735139));
#18398=CARTESIAN_POINT('Ctrl Pts',(-0.172453725526818,0.0138065207282529,
0.50829875985792));
#18399=CARTESIAN_POINT('Ctrl Pts',(-0.105064221167447,-0.137449688588867,
0.516240927980699));
#18400=CARTESIAN_POINT('Ctrl Pts',(0.0585749034388466,-0.162787862415564,
0.52418309610348));
#18401=CARTESIAN_POINT('Ctrl Pts',(0.168553398866689,-0.0389956304370821,
0.532125264226259));
#18402=CARTESIAN_POINT('Ctrl Pts',(0.124119664784058,0.120520605195094,
0.54006743234904));
#18403=CARTESIAN_POINT('Ctrl Pts',(-0.0340204335384149,0.16962758491636,
0.548009600471819));
#18404=CARTESIAN_POINT('Ctrl Pts',(-0.160994319687769,0.0633382703503284,
0.5559517685946));
#18405=CARTESIAN_POINT('Ctrl Pts',(-0.14048086942825,-0.100975406844349,
0.563893936717379));
#18406=CARTESIAN_POINT('Ctrl Pts',(0.00872748937560605,-0.172785237771916,
0.57183610484016));
#18407=CARTESIAN_POINT('Ctrl Pts',(0.149940571302356,-0.0863060399984934,
0.579778272962939));
#18408=CARTESIAN_POINT('Ctrl Pts',(0.153792685935992,0.0792383569699183,
0.58772044108572));
#18409=CARTESIAN_POINT('Ctrl Pts',(0.0167549005293281,0.17219227848818,
0.595662609208499));
#18410=CARTESIAN_POINT('Ctrl Pts',(-0.135632095058532,0.107400382926376,
0.60360477733128));
#18411=CARTESIAN_POINT('Ctrl Pts',(-0.163766157558233,-0.0557812970565469,
0.611546945454059));
#18412=CARTESIAN_POINT('Ctrl Pts',(-0.0418735953979919,-0.167861578305293,
0.61948911357684));
#18413=CARTESIAN_POINT('Ctrl Pts',(0.118379481984711,-0.126163408751231,
0.627431281699619));
#18414=CARTESIAN_POINT('Ctrl Pts',(0.17018479228316,0.0311134044783985,
0.6353734498224));
#18415=CARTESIAN_POINT('Ctrl Pts',(0.0660833491022344,0.159887142804326,
0.643315617945179));
#18416=CARTESIAN_POINT('Ctrl Pts',(-0.0985572308567358,0.142187832491218,
0.651257786067961));
#18417=CARTESIAN_POINT('Ctrl Pts',(-0.172909262181909,-0.00577013989488307,
0.659199954190738));
#18418=CARTESIAN_POINT('Ctrl Pts',(-0.0888586457050277,-0.148442071348278,
0.667142122313521));
#18419=CARTESIAN_POINT('Ctrl Pts',(0.0765956190331784,-0.155125815413241,
0.675084290436298));
#18420=CARTESIAN_POINT('Ctrl Pts',(0.171880427770071,-0.0196983758791502,
0.683026458559081));
#18421=CARTESIAN_POINT('Ctrl Pts',(0.109705106722326,0.133774799651286,
0.690968626681858));
#18422=CARTESIAN_POINT('Ctrl Pts',(-0.0529713625168984,0.164696515493808,
0.698910794804641));
#18423=CARTESIAN_POINT('Ctrl Pts',(-0.167120621735807,0.0447393032280997,
0.706852962927418));
#18424=CARTESIAN_POINT('Ctrl Pts',(-0.12817022249092,-0.116203707037801,
0.7147951310502));
#18425=CARTESIAN_POINT('Ctrl Pts',(0.0281972679828983,-0.17069218359667,
0.722737299172979));
#18426=CARTESIAN_POINT('Ctrl Pts',(0.158733164168978,-0.0688090841067,0.73067946729576));
#18427=CARTESIAN_POINT('Ctrl Pts',(0.14385317469873,0.0961102054508026,
0.738621635418538));
#18428=CARTESIAN_POINT('Ctrl Pts',(-0.00281110139369983,0.172982673038814,
0.746563803541321));
#18429=CARTESIAN_POINT('Ctrl Pts',(-0.146900119814081,0.0913852409380608,
0.754505971664098));
#18430=CARTESIAN_POINT('Ctrl Pts',(-0.156413536862055,-0.0739304602244656,
0.762448139786881));
#18431=CARTESIAN_POINT('Ctrl Pts',(-0.0226360851712103,-0.171518264656626,
0.770390307909658));
#18432=CARTESIAN_POINT('Ctrl Pts',(0.131878346029848,-0.111977717922496,
0.778332476032441));
#18433=CARTESIAN_POINT('Ctrl Pts',(0.165578663890314,0.0501459223366878,
0.786274644155218));
#18434=CARTESIAN_POINT('Ctrl Pts',(0.047591915084802,0.166330746049129,
0.794216812278001));
#18435=CARTESIAN_POINT('Ctrl Pts',(-0.113993917241593,0.130139518573781,
0.802158980400778));
#18436=CARTESIAN_POINT('Ctrl Pts',(-0.171149610334614,-0.0252728776558711,
0.81010114852356));
#18437=CARTESIAN_POINT('Ctrl Pts',(-0.0715146774936035,-0.157532721571376,
0.818043316646339));
#18438=CARTESIAN_POINT('Ctrl Pts',(0.0936350469135118,-0.14547640857611,
0.825985484769119));
#18439=CARTESIAN_POINT('Ctrl Pts',(0.173005448853992,-0.000148759965830227,
0.8339276528919));
#18440=CARTESIAN_POINT('Ctrl Pts',(0.0938850861191564,0.145315168055841,
0.841869821014678));
#18441=CARTESIAN_POINT('Ctrl Pts',(-0.0712436606821878,0.157655473343934,
0.849811989137461));
#18442=CARTESIAN_POINT('Ctrl Pts',(-0.171105895159299,0.0255671684868261,
0.857754157260238));
#18443=CARTESIAN_POINT('Ctrl Pts',(-0.114217551294,-0.129943289319231,0.86569632538302));
#18444=CARTESIAN_POINT('Ctrl Pts',(0.0473058035714782,-0.166412344527548,
0.873638493505798));
#18445=CARTESIAN_POINT('Ctrl Pts',(0.16549218245563,-0.0504305959589149,
0.88158066162858));
#18446=CARTESIAN_POINT('Ctrl Pts',(0.132070720552549,0.111750759440056,
0.889522829751358));
#18447=CARTESIAN_POINT('Ctrl Pts',(-0.022341089517305,0.171556938600217,
0.89746499787414));
#18448=CARTESIAN_POINT('Ctrl Pts',(-0.156286166401977,0.074199337288632,
0.905407165996919));
#18449=CARTESIAN_POINT('Ctrl Pts',(-0.147057058974526,-0.0911324797668838,
0.913349334119699));
#18450=CARTESIAN_POINT('Ctrl Pts',(-0.00310857778072832,-0.172977582960567,
0.92129150224248));
#18451=CARTESIAN_POINT('Ctrl Pts',(0.143687680016546,-0.0963574495000853,
0.929233670365259));
#18452=CARTESIAN_POINT('Ctrl Pts',(0.158851261322436,0.0685360068793772,
0.93717583848804));
#18453=CARTESIAN_POINT('Ctrl Pts',(0.0284907678468484,0.170643439985825,
0.945118006610819));
#18454=CARTESIAN_POINT('Ctrl Pts',(-0.127970195944242,0.116423951198588,
0.9530601747336));
#18455=CARTESIAN_POINT('Ctrl Pts',(-0.167197313372666,-0.0444518375735043,
0.961002342856378));
#18456=CARTESIAN_POINT('Ctrl Pts',(-0.0532545149190986,-0.164605176417482,
0.96894451097916));
#18457=CARTESIAN_POINT('Ctrl Pts',(0.10947489024455,-0.133963263130763,
0.976886679101939));
#18458=CARTESIAN_POINT('Ctrl Pts',(0.1719140491614,0.0194027617526574,0.984828847224719));
#18459=CARTESIAN_POINT('Ctrl Pts',(0.0768622776450996,0.154993863549195,
0.992771015347499));
#18460=CARTESIAN_POINT('Ctrl Pts',(-0.088603236555915,0.148594663210074,
1.00071318347028));
#18461=CARTESIAN_POINT('Ctrl Pts',(-0.172899083515371,0.00606748566075909,
1.00865535159306));
#18462=CARTESIAN_POINT('Ctrl Pts',(-0.0988016073770141,-0.142018132090297,
1.01659751971584));
#18463=CARTESIAN_POINT('Ctrl Pts',(0.0658082913934689,-0.160000550769587,
1.02453968783862));
#18464=CARTESIAN_POINT('Ctrl Pts',(0.170131034504888,-0.0314060274628177,
1.0324818559614));
#18465=CARTESIAN_POINT('Ctrl Pts',(0.118596271784576,0.125959643463681,
1.04042402408418));
#18466=CARTESIAN_POINT('Ctrl Pts',(-0.0415848597483297,0.167933340651612,
1.04836619220696));
#18467=CARTESIAN_POINT('Ctrl Pts',(-0.163669987576804,0.0560628453550813,
1.05630836032974));
#18468=CARTESIAN_POINT('Ctrl Pts',(-0.135816592328243,-0.107166975841641,
1.06425052845252));
#18469=CARTESIAN_POINT('Ctrl Pts',(0.0164587544616562,-0.172220837485682,
1.0721926965753));
#18470=CARTESIAN_POINT('Ctrl Pts',(0.153656191292587,-0.0795027190739688,
1.08013486469808));
#18471=CARTESIAN_POINT('Ctrl Pts',(0.150088771199207,0.0860480576341552,
1.08807703282086));
#18472=CARTESIAN_POINT('Ctrl Pts',(0.00902461748204118,0.172769973496559,
1.09601920094364));
#18473=CARTESIAN_POINT('Ctrl Pts',(-0.140307012982855,0.101216844302358,
1.10396136906642));
#18474=CARTESIAN_POINT('Ctrl Pts',(-0.161103005268346,-0.0630613126743013,
1.1119035371892));
#18475=CARTESIAN_POINT('Ctrl Pts',(-0.0343120939874615,-0.1695688287065,
1.11984570531198));
#18476=CARTESIAN_POINT('Ctrl Pts',(0.123912220401285,-0.120733877175888,
1.12778787343476));
#18477=CARTESIAN_POINT('Ctrl Pts',(0.168620210916381,0.0387057093103061,
1.13573004155754));
#18478=CARTESIAN_POINT('Ctrl Pts',(0.0588547652196237,0.162686889679659,
1.14367220968032));
#18479=CARTESIAN_POINT('Ctrl Pts',(-0.104827691798069,0.137630165643247,
1.1516143778031));
#18480=CARTESIAN_POINT('Ctrl Pts',(-0.172477213770776,-0.0135099294065116,
1.15955654592588));
#18481=CARTESIAN_POINT('Ctrl Pts',(-0.0821198886720452,-0.152273541192125,
1.16749871404866));
#18482=CARTESIAN_POINT('Ctrl Pts',(0.083467690946984,-0.15153894559049,
1.17544088217144));
#18483=CARTESIAN_POINT('Ctrl Pts',(0.172590290696882,-0.0119791076405788,
1.18338305029422));
#18484=CARTESIAN_POINT('Ctrl Pts',(0.103602453294194,0.13855482356859,1.191325218417));
#18485=CARTESIAN_POINT('Ctrl Pts',(-0.0602958748103966,0.162158302111078,
1.19926738653978));
#18486=CARTESIAN_POINT('Ctrl Pts',(-0.168956987158091,0.0372081167644847,
1.20720955466256));
#18487=CARTESIAN_POINT('Ctrl Pts',(-0.122836141658186,-0.121828526073448,
1.21515172278534));
#18488=CARTESIAN_POINT('Ctrl Pts',(0.0358152290369173,-0.169257723108079,
1.22309389090812));
#18489=CARTESIAN_POINT('Ctrl Pts',(0.161656170495932,-0.0616294572691503,
1.2310360590309));
#18490=CARTESIAN_POINT('Ctrl Pts',(0.13940345221127,0.102457722863032,1.23897822715368));
#18491=CARTESIAN_POINT('Ctrl Pts',(-0.0105571497596809,0.172683102970871,
1.24692039527646));
#18492=CARTESIAN_POINT('Ctrl Pts',(-0.150846317973597,0.0847130203482025,
1.25486256339924));
#18493=CARTESIAN_POINT('Ctrl Pts',(-0.152944761892581,-0.0808628918127005,
1.26280473152202));
#18494=CARTESIAN_POINT('Ctrl Pts',(-0.0149300913057054,-0.172360087712588,
1.2707468996448));
#18495=CARTESIAN_POINT('Ctrl Pts',(0.136762076743997,-0.105957736043287,
1.27868906776758));
#18496=CARTESIAN_POINT('Ctrl Pts',(0.163166132393764,0.0575127872937276,
1.28663123589036));
#18497=CARTESIAN_POINT('Ctrl Pts',(0.0400932480780463,0.168295688956082,
1.29457340401314));
#18498=CARTESIAN_POINT('Ctrl Pts',(-0.119709170414695,0.124902449862528,
1.30251557213592));
#18499=CARTESIAN_POINT('Ctrl Pts',(-0.169845690614082,-0.0329142650230248,
1.3104577402587));
#18500=CARTESIAN_POINT('Ctrl Pts',(-0.0643861093061943,-0.160578131733314,
1.31839990838148));
#18501=CARTESIAN_POINT('Ctrl Pts',(0.100057762773863,-0.141135932963798,
1.32634207650426));
#18502=CARTESIAN_POINT('Ctrl Pts',(0.172838444806952,0.00760127985757451,
1.33428424462704));
#18503=CARTESIAN_POINT('Ctrl Pts',(0.0872813550697656,0.149374939398002,
1.34222641274982));
#18504=CARTESIAN_POINT('Ctrl Pts',(-0.0782344227434143,0.154305808621531,
1.3501685808726));
#18505=CARTESIAN_POINT('Ctrl Pts',(-0.172079431848303,0.0178767046294837,
1.35811074899538));
#18506=CARTESIAN_POINT('Ctrl Pts',(-0.108282003268856,-0.134929297194493,
1.36605291711816));
#18507=CARTESIAN_POINT('Ctrl Pts',(0.0547128650701426,-0.164126201264144,
1.37399508524094));
#18508=CARTESIAN_POINT('Ctrl Pts',(0.167585127127835,-0.0429666431014547,
1.38193725336372));
#18509=CARTESIAN_POINT('Ctrl Pts',(0.126932197981417,0.117554773230619,
1.3898794214865));
#18510=CARTESIAN_POINT('Ctrl Pts',(-0.0300036684000219,0.170383942402052,
1.39782158960928));
#18511=CARTESIAN_POINT('Ctrl Pts',(-0.159453085214751,0.0671239123677834,
1.40576375773206));
#18512=CARTESIAN_POINT('Ctrl Pts',(-0.142827107870127,-0.0976285101620078,
1.41370592585484));
#18513=CARTESIAN_POINT('Ctrl Pts',(0.00464319840846943,-0.172943201171859,
1.42164809397762));
#18514=CARTESIAN_POINT('Ctrl Pts',(0.147859810582222,-0.0898241270588577,
1.4295902621004));
#18515=CARTESIAN_POINT('Ctrl Pts',(0.155621735944117,0.0755830265922534,
1.43753243022318));
#18516=CARTESIAN_POINT('Ctrl Pts',(0.0208179928734729,0.171748455656582,
1.44547459834596));
#18517=CARTESIAN_POINT('Ctrl Pts',(-0.133056846329205,0.11057447892796,
1.45341676646874));
#18518=CARTESIAN_POINT('Ctrl Pts',(-0.165038560097216,-0.0518967460486161,
1.46135893459152));
#18519=CARTESIAN_POINT('Ctrl Pts',(-0.0458268296361176,-0.166825854601292,
1.4693011027143));
#18520=CARTESIAN_POINT('Ctrl Pts',(0.115364766925686,-0.128924136976022,
1.47724327083708));
#18521=CARTESIAN_POINT('Ctrl Pts',(0.170874595884426,0.0270830477535184,
1.48518543895986));
#18522=CARTESIAN_POINT('Ctrl Pts',(0.0698377457337486,0.158283721017069,
1.49312760708264));
#18523=CARTESIAN_POINT('Ctrl Pts',(-0.0951624750893037,0.144471999488883,
1.50106977520542));
#18524=CARTESIAN_POINT('Ctrl Pts',(-0.173012914651864,-0.00167525885548286,
1.5090119433282));
#18525=CARTESIAN_POINT('Ctrl Pts',(-0.092311001583214,-0.14631755460685,
1.51695411145098));
#18526=CARTESIAN_POINT('Ctrl Pts',(0.072853104778531,-0.156861289272697,
1.52489627957376));
#18527=CARTESIAN_POINT('Ctrl Pts',(0.171475934783304,-0.0238129810547936,
1.53283844769654));
#18528=CARTESIAN_POINT('Ctrl Pts',(0.11261423476106,0.131269690464983,1.54078061581932));
#18529=CARTESIAN_POINT('Ctrl Pts',(0.00518264413773371,0.154149172621267,
1.54607539456784));
#18530=CARTESIAN_POINT('Ctrl Pts',(-0.0415060733757155,0.140340900570467,
1.5487227839421));
#18531=CARTESIAN_POINT('Ctrl Pts',(-0.146248097568756,-0.000123763188177425,
1.45893449541571));
#18532=CARTESIAN_POINT('Ctrl Pts',(-0.146367493381718,-0.0150081347743067,
1.45974264180765));
#18533=CARTESIAN_POINT('Ctrl Pts',(-0.144277648885518,-0.0298597803798721,
1.46055078819958));
#18534=CARTESIAN_POINT('Ctrl Pts',(-0.139839652725699,-0.043973059977961,
1.46135893459152));
#18535=CARTESIAN_POINT('Ctrl Pts',(-0.125301316610186,-0.0902064488995044,
1.46400632396578));
#18536=CARTESIAN_POINT('Ctrl Pts',(-0.08556407312315,-0.1285161517504,1.46665371334004));
#18537=CARTESIAN_POINT('Ctrl Pts',(-0.0388301852859989,-0.141354050238301,
1.4693011027143));
#18538=CARTESIAN_POINT('Ctrl Pts',(0.00790370255115092,-0.154191948726202,
1.47194849208856));
#18539=CARTESIAN_POINT('Ctrl Pts',(0.0616342347384179,-0.141558042851112,
1.47459588146282));
#18540=CARTESIAN_POINT('Ctrl Pts',(0.0977511389918415,-0.109239892458645,
1.47724327083708));
#18541=CARTESIAN_POINT('Ctrl Pts',(0.133868043245265,-0.0769217420661769,
1.47989066021134));
#18542=CARTESIAN_POINT('Ctrl Pts',(0.152371319564846,-0.024919347156331,
1.4825380495856));
#18543=CARTESIAN_POINT('Ctrl Pts',(0.144783482699524,0.0229486291758506,
1.48518543895986));
#18544=CARTESIAN_POINT('Ctrl Pts',(0.137195645834202,0.0708166055080336,
1.48783282833412));
#18545=CARTESIAN_POINT('Ctrl Pts',(0.103516695783975,0.114550163262552,
1.49048021770838));
#18546=CARTESIAN_POINT('Ctrl Pts',(0.0591771839550196,0.13411498855178,
1.49312760708264));
#18547=CARTESIAN_POINT('Ctrl Pts',(0.014837672126065,0.153679813841007,
1.4957749964569));
#18548=CARTESIAN_POINT('Ctrl Pts',(-0.0401624014816186,0.149075906664945,
1.49842238583116));
#18549=CARTESIAN_POINT('Ctrl Pts',(-0.0806375115458872,0.122416076686187,
1.50106977520542));
#18550=CARTESIAN_POINT('Ctrl Pts',(-0.0937869288003098,0.113754921033589,
1.50192985013695));
#18551=CARTESIAN_POINT('Ctrl Pts',(-0.105403311347291,0.102765876910903,
1.50278992506847));
#18552=CARTESIAN_POINT('Ctrl Pts',(-0.115078604842433,0.0902138214954038,
1.50365));
#18553=CARTESIAN_POINT('Ctrl Pts',(-0.0686146973663081,-0.0959584553529135,
1.07336015076065E-17));
#18554=CARTESIAN_POINT('Ctrl Pts',(-0.0712979561985307,-0.0944995001033786,
9.02613639135873E-18));
#18555=CARTESIAN_POINT('Ctrl Pts',(-0.0739152333025289,-0.0929325179580126,
1.64107321374712E-17));
#18556=CARTESIAN_POINT('Ctrl Pts',(-0.0764591723283171,-0.0912589988675934,
1.6154612370034E-17));
#18557=CARTESIAN_POINT('Ctrl Pts',(-0.0824897891353913,-0.0872917841461184,
1.52077426268717E-17));
#18558=CARTESIAN_POINT('Ctrl Pts',(-0.0881090519769445,-0.0827275518978924,
1.30971627060498E-17));
#18559=CARTESIAN_POINT('Ctrl Pts',(-0.0932912133381108,-0.0776621329443405,
1.43114686768087E-17));
#18560=CARTESIAN_POINT('Ctrl Pts',(-0.0960634919631888,-0.074952307504085,
1.49610807310118E-17));
#18561=CARTESIAN_POINT('Ctrl Pts',(-0.0987043519497191,-0.0721043812799658,
1.74993329480528E-17));
#18562=CARTESIAN_POINT('Ctrl Pts',(-0.101206237074718,-0.0691378820326018,
9.97465998686664E-18));
#18563=CARTESIAN_POINT('Ctrl Pts',(-0.105823426721714,-0.0636632543305198,
-3.91200561030858E-18));
#18564=CARTESIAN_POINT('Ctrl Pts',(-0.109972666997065,-0.0577811896139199,
2.24798207762934E-18));
#18565=CARTESIAN_POINT('Ctrl Pts',(-0.113625452403263,-0.0515741981665521,
9.54097911787244E-18));
#18566=CARTESIAN_POINT('Ctrl Pts',(-0.115386295340069,-0.0485820878086944,
1.30566037435822E-17));
#18567=CARTESIAN_POINT('Ctrl Pts',(-0.117027309103105,-0.0455212415157476,
-2.79521757168051E-18));
#18568=CARTESIAN_POINT('Ctrl Pts',(-0.118543833519887,-0.0424058589801268,
-3.46944695195361E-18));
#18569=CARTESIAN_POINT('Ctrl Pts',(-0.122700941917732,-0.0338659484069709,
-5.31764971597768E-18));
#18570=CARTESIAN_POINT('Ctrl Pts',(-0.125931492798984,-0.0249085743588085,
-1.15219401683824E-18));
#18571=CARTESIAN_POINT('Ctrl Pts',(-0.128167520083254,-0.0157105262534848,
9.54097911787244E-18));
#18572=CARTESIAN_POINT('Ctrl Pts',(-0.128992166906242,-0.0123182862745252,
1.3484621181291E-17));
#18573=CARTESIAN_POINT('Ctrl Pts',(-0.129681150280034,-0.00889298553317688,
1.10989611676181E-17));
#18574=CARTESIAN_POINT('Ctrl Pts',(-0.130229483957028,-0.00544263935519351,
9.54097911787244E-18));
#18575=CARTESIAN_POINT('Ctrl Pts',(-0.130761899349706,-0.00209245771889707,
8.02822573502553E-18));
#18576=CARTESIAN_POINT('Ctrl Pts',(-0.131160261982709,0.00127366115726457,
1.11791151702242E-17));
#18577=CARTESIAN_POINT('Ctrl Pts',(-0.131420990891747,0.00464012593483382,
8.67361737988404E-18));
#18578=CARTESIAN_POINT('Ctrl Pts',(-0.131728666658755,0.00861275649723166,
5.71697955546795E-18));
#18579=CARTESIAN_POINT('Ctrl Pts',(-0.131845259942619,0.0125891451047215,
-9.26473565962443E-18));
#18580=CARTESIAN_POINT('Ctrl Pts',(-0.131765781147177,0.0165567997877194,
-1.04083408558608E-17));
#18581=CARTESIAN_POINT('Ctrl Pts',(-0.131635692412819,0.0230509492424239,
-1.21888544026837E-17));
#18582=CARTESIAN_POINT('Ctrl Pts',(-0.13098103789945,0.0295216962360144,
-2.67049856555875E-17));
#18583=CARTESIAN_POINT('Ctrl Pts',(-0.129839098367345,0.0359278479980343,
-3.46944695195361E-17));
#18584=CARTESIAN_POINT('Ctrl Pts',(-0.129254890951344,0.0392051855997028,
-3.87818275556788E-17));
#18585=CARTESIAN_POINT('Ctrl Pts',(-0.128542951403208,0.0424656461998481,
-3.10678831811161E-17));
#18586=CARTESIAN_POINT('Ctrl Pts',(-0.1277070993652,0.0457037274559979,
-3.29597460435593E-17));
#18587=CARTESIAN_POINT('Ctrl Pts',(-0.126886363095037,0.0488832504000222,
-3.48173959609792E-17));
#18588=CARTESIAN_POINT('Ctrl Pts',(-0.125948031872817,0.0520333657183593,
-3.53366201082739E-17));
#18589=CARTESIAN_POINT('Ctrl Pts',(-0.124899042599898,0.0551436241923499,
-3.46944695195361E-17));
#18590=CARTESIAN_POINT('Ctrl Pts',(-0.122234979928128,0.0630425834229368,
-3.30636335736642E-17));
#18591=CARTESIAN_POINT('Ctrl Pts',(-0.118856305871375,0.070695441500891,
-2.1366080483524E-17));
#18592=CARTESIAN_POINT('Ctrl Pts',(-0.114834854776346,0.078019637496205,
-1.73472347597681E-17));
#18593=CARTESIAN_POINT('Ctrl Pts',(-0.11215901866562,0.0828930893082948,
-1.46731322388254E-17));
#18594=CARTESIAN_POINT('Ctrl Pts',(-0.109198005187061,0.0876211033078822,
8.28606628989234E-18));
#18595=CARTESIAN_POINT('Ctrl Pts',(-0.105966883726074,0.0921780034666525,
8.67361737988404E-18));
#18596=CARTESIAN_POINT('Ctrl Pts',(-0.104137243112614,0.094758373688769,
8.89307035390601E-18));
#18597=CARTESIAN_POINT('Ctrl Pts',(-0.102221042121924,0.0972831505018574,
-2.31209379389524E-17));
#18598=CARTESIAN_POINT('Ctrl Pts',(-0.100229777791505,0.0997373632832089,
-2.08166817117217E-17));
#18599=CARTESIAN_POINT('Ctrl Pts',(-0.0937202782075859,0.107760254486057,
-1.32840027382311E-17));
#18600=CARTESIAN_POINT('Ctrl Pts',(-0.0863914655699752,0.115060936709644,
5.4842312373535E-18));
#18601=CARTESIAN_POINT('Ctrl Pts',(-0.0783508402622743,0.121487309774744,
1.38777878078145E-17));
#18602=CARTESIAN_POINT('Ctrl Pts',(-0.073610711791116,0.125275800441382,
1.8825977152717E-17));
#18603=CARTESIAN_POINT('Ctrl Pts',(-0.068622257850438,0.128760167547443,
-9.09579695168528E-18));
#18604=CARTESIAN_POINT('Ctrl Pts',(-0.0634007094575209,0.131904027763685,
-6.93889390390723E-18));
#18605=CARTESIAN_POINT('Origin',(0.,0.,0.));
#18606=CARTESIAN_POINT('Origin',(-0.0721687836487033,-0.125,-0.3));
#18607=CARTESIAN_POINT('',(-0.0721687836487033,-0.125,-0.3));
#18608=CARTESIAN_POINT('',(0.0721687836487032,-0.125,-0.3));
#18609=CARTESIAN_POINT('',(-0.0360843918243517,-0.125,-0.3));
#18610=CARTESIAN_POINT('',(-0.0721687836487033,-0.125,-0.15));
#18611=CARTESIAN_POINT('',(-0.0721687836487033,-0.125,-0.3));
#18612=CARTESIAN_POINT('',(0.0721687836487032,-0.125,-0.15));
#18613=CARTESIAN_POINT('',(-0.0721687836487033,-0.125,-0.15));
#18614=CARTESIAN_POINT('',(0.0721687836487032,-0.125,-0.3));
#18615=CARTESIAN_POINT('Origin',(-0.144337567297406,1.76762539787485E-17,
-0.3));
#18616=CARTESIAN_POINT('',(-0.144337567297406,1.76762539787485E-17,-0.3));
#18617=CARTESIAN_POINT('',(-0.126295371385231,-0.03125,-0.3));
#18618=CARTESIAN_POINT('',(-0.144337567297406,2.77555756156289E-17,-0.15));
#18619=CARTESIAN_POINT('',(-0.144337567297406,1.76762539787485E-17,-0.3));
#18620=CARTESIAN_POINT('',(-0.144337567297406,1.76762539787485E-17,-0.15));
#18621=CARTESIAN_POINT('Origin',(-0.0721687836487032,0.125,-0.3));
#18622=CARTESIAN_POINT('',(-0.0721687836487032,0.125,-0.3));
#18623=CARTESIAN_POINT('',(-0.090210979560879,0.09375,-0.3));
#18624=CARTESIAN_POINT('',(-0.0721687836487032,0.125,-0.15));
#18625=CARTESIAN_POINT('',(-0.0721687836487032,0.125,-0.3));
#18626=CARTESIAN_POINT('',(-0.0721687836487032,0.125,-0.15));
#18627=CARTESIAN_POINT('Origin',(0.0721687836487032,0.125,-0.3));
#18628=CARTESIAN_POINT('',(0.0721687836487032,0.125,-0.3));
#18629=CARTESIAN_POINT('',(0.0360843918243516,0.125,-0.3));
#18630=CARTESIAN_POINT('',(0.0721687836487032,0.125,-0.15));
#18631=CARTESIAN_POINT('',(0.0721687836487032,0.125,-0.3));
#18632=CARTESIAN_POINT('',(0.0721687836487032,0.125,-0.15));
#18633=CARTESIAN_POINT('Origin',(0.144337567297406,0.,-0.3));
#18634=CARTESIAN_POINT('',(0.144337567297406,0.,-0.3));
#18635=CARTESIAN_POINT('',(0.126295371385231,0.03125,-0.3));
#18636=CARTESIAN_POINT('',(0.144337567297406,0.,-0.15));
#18637=CARTESIAN_POINT('',(0.144337567297406,0.,-0.3));
#18638=CARTESIAN_POINT('',(0.144337567297406,0.,-0.15));
#18639=CARTESIAN_POINT('Origin',(0.0721687836487032,-0.125,-0.3));
#18640=CARTESIAN_POINT('',(0.0902109795608791,-0.09375,-0.3));
#18641=CARTESIAN_POINT('',(0.0721687836487032,-0.125,-0.15));
#18642=CARTESIAN_POINT('Origin',(0.,0.,-0.15));
#18643=CARTESIAN_POINT('Origin',(0.,0.,0.));
#18644=CARTESIAN_POINT('',(-0.275,-3.36777869765522E-17,0.));
#18645=CARTESIAN_POINT('Origin',(0.,0.,0.));
#18646=CARTESIAN_POINT('Origin',(0.,0.,-0.3));
#18647=CARTESIAN_POINT('',(-0.275,-3.36777869765522E-17,-0.3));
#18648=CARTESIAN_POINT('',(-0.275,-3.36777869765522E-17,-0.3));
#18649=CARTESIAN_POINT('Origin',(0.,0.,-0.3));
#18650=CARTESIAN_POINT('Origin',(0.,0.,-0.3));
#18651=CARTESIAN_POINT('Origin',(0.,0.,1.6));
#18652=CARTESIAN_POINT('',(0.,0.,0.));
#18653=CARTESIAN_POINT('Origin',(0.,0.,0.12));
#18654=CARTESIAN_POINT('',(-0.12639138516214,8.91322620741042E-5,0.00934196736194174));
#18655=CARTESIAN_POINT('',(-0.12645,1.54856587752183E-17,-5.55111512312578E-17));
#18656=CARTESIAN_POINT('',(-0.12645,1.54856587752183E-17,0.12));
#18657=CARTESIAN_POINT('',(-0.0488748409397564,0.116622692573588,0.));
#18658=CARTESIAN_POINT('Origin',(0.,0.,0.));
#18659=CARTESIAN_POINT('Ctrl Pts',(-0.0489111879062984,0.116810626195002,
1.20007714660797E-17));
#18660=CARTESIAN_POINT('Ctrl Pts',(-0.0838963038512042,0.101957324585112,
0.00240024091002088));
#18661=CARTESIAN_POINT('Ctrl Pts',(-0.11198221847721,0.0702793053867637,
0.00480048182004174));
#18662=CARTESIAN_POINT('Ctrl Pts',(-0.122072221370749,0.0336561163696377,
0.00720072273006261));
#18663=CARTESIAN_POINT('Ctrl Pts',(-0.125072637487486,0.022765653033531,
0.00791447094068899));
#18664=CARTESIAN_POINT('Ctrl Pts',(-0.126481745582665,0.0114379076904012,
0.00862821915131536));
#18665=CARTESIAN_POINT('Ctrl Pts',(-0.12639138516214,8.91322620741042E-5,
0.00934196736194174));
#18666=CARTESIAN_POINT('Origin',(0.,0.,0.12));
#18667=CARTESIAN_POINT('',(-0.126396145829628,-9.95859796292312E-5,0.0593419673619417));
#18668=CARTESIAN_POINT('',(-0.126575671592806,-7.20628672610732E-5,0.0456580326380584));
#18669=CARTESIAN_POINT('',(-0.12645,1.54856587752183E-17,0.12));
#18670=CARTESIAN_POINT('',(-0.10808967569503,-0.0656218295092665,0.));
#18671=CARTESIAN_POINT('Ctrl Pts',(-0.126575671592806,-7.20628672610732E-5,
0.0456580326380584));
#18672=CARTESIAN_POINT('Ctrl Pts',(-0.126327459688109,0.0361497101693465,
0.0433719816070355));
#18673=CARTESIAN_POINT('Ctrl Pts',(-0.109912066394173,0.0725710138228805,
0.0410859305760125));
#18674=CARTESIAN_POINT('Ctrl Pts',(-0.0824515099939393,0.0961223418729112,
0.0387998795449896));
#18675=CARTESIAN_POINT('Ctrl Pts',(-0.05137998778939,0.122770586059505,
0.036213220908657));
#18676=CARTESIAN_POINT('Ctrl Pts',(-0.00616751748104999,0.132941603485868,
0.0336265622723243));
#18677=CARTESIAN_POINT('Ctrl Pts',(0.0333172074018229,0.122176268745047,
0.0310399036359917));
#18678=CARTESIAN_POINT('Ctrl Pts',(0.0728019322846963,0.111410934004226,
0.028453244999659));
#18679=CARTESIAN_POINT('Ctrl Pts',(0.106558911742102,0.0797092470962188,
0.0258665863633264));
#18680=CARTESIAN_POINT('Ctrl Pts',(0.11981357554495,0.0409763259700822,
0.0232799277269937));
#18681=CARTESIAN_POINT('Ctrl Pts',(0.133068239347797,0.00224340484394604,
0.0206932690906611));
#18682=CARTESIAN_POINT('Ctrl Pts',(0.125820587496086,-0.0435207505003201,
0.0181066104543285));
#18683=CARTESIAN_POINT('Ctrl Pts',(0.101166903546451,-0.0762076816581678,
0.0155199518179958));
#18684=CARTESIAN_POINT('Ctrl Pts',(0.0765132195968157,-0.108894612816016,
0.0129332931816632));
#18685=CARTESIAN_POINT('Ctrl Pts',(0.0344535035492562,-0.128504319787445,
0.0103466345453306));
#18686=CARTESIAN_POINT('Ctrl Pts',(-0.00636464094143544,-0.126469737202777,
0.00775997590899791));
#18687=CARTESIAN_POINT('Ctrl Pts',(-0.0471827854321269,-0.124435154618108,
0.00517331727266527));
#18688=CARTESIAN_POINT('Ctrl Pts',(-0.0867593583659505,-0.100756282477341,
0.00258665863633259));
#18689=CARTESIAN_POINT('Ctrl Pts',(-0.108089675695031,-0.0656218295092657,
-5.55111512312578E-17));
#18690=CARTESIAN_POINT('Origin',(0.,0.,0.));
#18691=CARTESIAN_POINT('Ctrl Pts',(-0.12639138516214,8.91322620741042E-5,
0.00934196736194174));
#18692=CARTESIAN_POINT('Ctrl Pts',(-0.126154274972366,-0.0296906128949183,
0.011214877787648));
#18693=CARTESIAN_POINT('Ctrl Pts',(-0.115592373032178,-0.0596151635265703,
0.0130877882133543));
#18694=CARTESIAN_POINT('Ctrl Pts',(-0.0963650578556872,-0.0821635787359664,
0.0149606986390606));
#18695=CARTESIAN_POINT('Ctrl Pts',(-0.0698103971670931,-0.113304978845907,
0.0175473572753932));
#18696=CARTESIAN_POINT('Ctrl Pts',(-0.0267272342632827,-0.130377059081323,
0.0201340159117258));
#18697=CARTESIAN_POINT('Ctrl Pts',(0.0139574509341311,-0.125868770046104,
0.0227206745480584));
#18698=CARTESIAN_POINT('Ctrl Pts',(0.0546421361315456,-0.121360481010885,
0.0253073331843911));
#18699=CARTESIAN_POINT('Ctrl Pts',(0.0929283436225635,-0.0952718227050311,
0.0278939918207237));
#18700=CARTESIAN_POINT('Ctrl Pts',(0.112018291148455,-0.0590635258734944,
0.0304806504570564));
#18701=CARTESIAN_POINT('Ctrl Pts',(0.131108238674346,-0.0228552290419586,
0.033067309093389));
#18702=CARTESIAN_POINT('Ctrl Pts',(0.131001926235112,0.0234727063152593,
0.0356539677297216));
#18703=CARTESIAN_POINT('Ctrl Pts',(0.111741771403992,0.0595891814911641,
0.0382406263660542));
#18704=CARTESIAN_POINT('Ctrl Pts',(0.0924816165728724,0.0957056566670696,
0.0408272850023869));
#18705=CARTESIAN_POINT('Ctrl Pts',(0.0540676193498672,0.121610671661662,
0.0434139436387195));
#18706=CARTESIAN_POINT('Ctrl Pts',(0.0133639835211523,0.125930636937597,
0.0460006022750522));
#18707=CARTESIAN_POINT('Ctrl Pts',(-0.0273396523075625,0.130250602213533,
0.0485872609113848));
#18708=CARTESIAN_POINT('Ctrl Pts',(-0.0703329267419868,0.112985517770812,
0.0511739195477175));
#18709=CARTESIAN_POINT('Ctrl Pts',(-0.0967449447385466,0.0817152626609385,
0.0537605781840501));
#18710=CARTESIAN_POINT('Ctrl Pts',(-0.115741878896724,0.0592240248649833,
0.0556210412433473));
#18711=CARTESIAN_POINT('Ctrl Pts',(-0.126160906676814,0.0294875554882879,
0.0574815043026445));
#18712=CARTESIAN_POINT('Ctrl Pts',(-0.126396145829628,-9.95859796292312E-5,
0.0593419673619417));
#18713=CARTESIAN_POINT('Origin',(0.,0.,0.12));
#18714=CARTESIAN_POINT('',(-0.126529791093031,9.025049583615E-5,0.109341967361942));
#18715=CARTESIAN_POINT('',(-0.126349242904067,8.85860673823967E-5,0.0956580326380584));
#18716=CARTESIAN_POINT('',(-0.12645,1.54856587752183E-17,0.12));
#18717=CARTESIAN_POINT('Ctrl Pts',(-0.126349242904067,8.85860673823967E-5,
0.0956580326380584));
#18718=CARTESIAN_POINT('Ctrl Pts',(-0.126441591528965,0.0135570965972842,
0.0948119253946973));
#18719=CARTESIAN_POINT('Ctrl Pts',(-0.124448136217638,0.0269990101701626,
0.0939658181513361));
#18720=CARTESIAN_POINT('Ctrl Pts',(-0.120249444863787,0.0397126388809939,
0.093119710907975));
#18721=CARTESIAN_POINT('Ctrl Pts',(-0.107413505522824,0.0785798365820317,
0.0905330522716423));
#18722=CARTESIAN_POINT('Ctrl Pts',(-0.0739673525896496,0.110640458354997,
0.0879463936353097));
#18723=CARTESIAN_POINT('Ctrl Pts',(-0.0345920580258737,0.121821308595361,
0.085359734998977));
#18724=CARTESIAN_POINT('Ctrl Pts',(0.00478323653790218,0.133002158835724,
0.0827730763626444));
#18725=CARTESIAN_POINT('Ctrl Pts',(0.0500876727322792,0.123303237543486,
0.0801864177263117));
#18726=CARTESIAN_POINT('Ctrl Pts',(0.0814342209129887,0.0969820390626645,
0.077599759089979));
#18727=CARTESIAN_POINT('Ctrl Pts',(0.112780769093698,0.0706608405818426,
0.0750131004536464));
#18728=CARTESIAN_POINT('Ctrl Pts',(0.13016942926074,0.0277173649124373,
0.0724264418173139));
#18729=CARTESIAN_POINT('Ctrl Pts',(0.12596827751407,-0.0129984006283456,
0.0698397831809812));
#18730=CARTESIAN_POINT('Ctrl Pts',(0.121767125767399,-0.0537141661691284,
0.0672531245446486));
#18731=CARTESIAN_POINT('Ctrl Pts',(0.0959761621070158,-0.0922022215812886,
0.0646664659083159));
#18732=CARTESIAN_POINT('Ctrl Pts',(0.059914723710966,-0.111567668284471,
0.0620798072719833));
#18733=CARTESIAN_POINT('Ctrl Pts',(0.0238532853149157,-0.130933114987654,
0.0594931486356506));
#18734=CARTESIAN_POINT('Ctrl Pts',(-0.0224786278168013,-0.131175952981858,
0.056906489999318));
#18735=CARTESIAN_POINT('Ctrl Pts',(-0.0587401909579078,-0.112190380850839,
0.0543198313629853));
#18736=CARTESIAN_POINT('Ctrl Pts',(-0.0950017540990138,-0.0932048087198191,
0.0517331727266527));
#18737=CARTESIAN_POINT('Ctrl Pts',(-0.12119296724951,-0.0549908264635757,
0.0491465140903201));
#18738=CARTESIAN_POINT('Ctrl Pts',(-0.125823286774378,-0.0143210998620416,
0.0465598554539874));
#18739=CARTESIAN_POINT('Ctrl Pts',(-0.126361397696569,-0.0095946821776348,
0.0462592478486778));
#18740=CARTESIAN_POINT('Ctrl Pts',(-0.12660831057823,-0.00483509759607578,
0.0459586402433681));
#18741=CARTESIAN_POINT('Ctrl Pts',(-0.126575671592806,-7.20628672610732E-5,
0.0456580326380584));
#18742=CARTESIAN_POINT('Ctrl Pts',(-0.126396145829628,-9.95859796292312E-5,
0.0593419673619417));
#18743=CARTESIAN_POINT('Ctrl Pts',(-0.12648796685852,-0.0116483513064931,
0.0600681629389771));
#18744=CARTESIAN_POINT('Ctrl Pts',(-0.125028206814926,-0.0231743653405588,
0.0607943585160125));
#18745=CARTESIAN_POINT('Ctrl Pts',(-0.121921363946098,-0.034237873926493,
0.0615205540930479));
#18746=CARTESIAN_POINT('Ctrl Pts',(-0.110855003598394,-0.0736453296270277,
0.0641072127293806));
#18747=CARTESIAN_POINT('Ctrl Pts',(-0.0788915213442898,-0.107184815251071,
0.0666938713657133));
#18748=CARTESIAN_POINT('Ctrl Pts',(-0.0400617348236378,-0.120133683626334,
0.069280530002046));
#18749=CARTESIAN_POINT('Ctrl Pts',(-0.00123194830298627,-0.133082552001597,
0.0718671886383786));
#18750=CARTESIAN_POINT('Ctrl Pts',(0.0444641424842127,-0.125440803128081,
0.0744538472747112));
#18751=CARTESIAN_POINT('Ctrl Pts',(0.0769682295152699,-0.100563001286921,
0.0770405059110438));
#18752=CARTESIAN_POINT('Ctrl Pts',(0.109472316546327,-0.0756851994457607,
0.0796271645473764));
#18753=CARTESIAN_POINT('Ctrl Pts',(0.128784399821243,-0.0335713446369571,
0.0822138231837091));
#18754=CARTESIAN_POINT('Ctrl Pts',(0.126427276285523,0.00729262199647547,
0.0848004818200417));
#18755=CARTESIAN_POINT('Ctrl Pts',(0.124070152749803,0.0481565886299079,
0.0873871404563744));
#18756=CARTESIAN_POINT('Ctrl Pts',(0.100043822403448,0.0877706670879697,
0.0899737990927071));
#18757=CARTESIAN_POINT('Ctrl Pts',(0.0648947831756147,0.108746049780439,
0.0925604577290397));
#18758=CARTESIAN_POINT('Ctrl Pts',(0.0297457439477817,0.129721432472907,
0.0951471163653723));
#18759=CARTESIAN_POINT('Ctrl Pts',(-0.0165260041615291,0.132058119399784,
0.0977337750017049));
#18760=CARTESIAN_POINT('Ctrl Pts',(-0.0536093211433369,0.114730442741844,
0.100320433638038));
#18761=CARTESIAN_POINT('Ctrl Pts',(-0.0906926381251451,0.0974027660839045,
0.10290709227437));
#18762=CARTESIAN_POINT('Ctrl Pts',(-0.11858752397945,0.0604107258411485,
0.105493750910703));
#18763=CARTESIAN_POINT('Ctrl Pts',(-0.12504939731921,0.0199921027543164,
0.108080409547035));
#18764=CARTESIAN_POINT('Ctrl Pts',(-0.126099919499473,0.0134211506765118,
0.108500928818671));
#18765=CARTESIAN_POINT('Ctrl Pts',(-0.126583971845017,0.00675963476331471,
0.108921448090306));
#18766=CARTESIAN_POINT('Ctrl Pts',(-0.126529791093031,9.025049583615E-5,
0.109341967361942));
#18767=CARTESIAN_POINT('Origin',(0.,0.,0.12));
#18768=CARTESIAN_POINT('',(-0.126296536029262,-6.10717992316628E-5,0.159341967361942));
#18769=CARTESIAN_POINT('',(-0.126453631260982,-0.000102348163238207,0.145658032638058));
#18770=CARTESIAN_POINT('',(-0.12645,1.54856587752183E-17,0.12));
#18771=CARTESIAN_POINT('Ctrl Pts',(-0.126453631260982,-0.000102348163238207,
0.145658032638058));
#18772=CARTESIAN_POINT('Ctrl Pts',(-0.126183364177612,0.031552920325249,
0.143665210546026));
#18773=CARTESIAN_POINT('Ctrl Pts',(-0.114073771100105,0.0633928690595716,
0.141672388453994));
#18774=CARTESIAN_POINT('Ctrl Pts',(-0.0925489356314354,0.0864391430514358,
0.139679566361962));
#18775=CARTESIAN_POINT('Ctrl Pts',(-0.0646099631645552,0.116352924063146,
0.13709290772563));
#18776=CARTESIAN_POINT('Ctrl Pts',(-0.0208084524006029,0.131451366650306,
0.134506249089297));
#18777=CARTESIAN_POINT('Ctrl Pts',(0.0196287675426836,0.125106932552633,
0.131919590452964));
#18778=CARTESIAN_POINT('Ctrl Pts',(0.0600659874859703,0.11876249845496,
0.129332931816632));
#18779=CARTESIAN_POINT('Ctrl Pts',(0.097138916608591,0.0909751876724545,
0.126746273180299));
#18780=CARTESIAN_POINT('Ctrl Pts',(0.114574233156503,0.0539423598350403,
0.124159614543967));
#18781=CARTESIAN_POINT('Ctrl Pts',(0.132009549704415,0.0169095319976262,
0.121572955907634));
#18782=CARTESIAN_POINT('Ctrl Pts',(0.129807253677619,-0.0293688128946969,
0.118986297271301));
#18783=CARTESIAN_POINT('Ctrl Pts',(0.108934072954415,-0.0645786240759305,
0.116399638634969));
#18784=CARTESIAN_POINT('Ctrl Pts',(0.0880608922312115,-0.099788435257164,
0.113812979998636));
#18785=CARTESIAN_POINT('Ctrl Pts',(0.0485168268116012,-0.123929712727308,
0.111226321362303));
#18786=CARTESIAN_POINT('Ctrl Pts',(0.00765986125275547,-0.126405537442516,
0.108639662725971));
#18787=CARTESIAN_POINT('Ctrl Pts',(-0.0331971043060904,-0.128881362157723,
0.106053004089638));
#18788=CARTESIAN_POINT('Ctrl Pts',(-0.0753669700041717,-0.109691734117994,
0.103466345453305));
#18789=CARTESIAN_POINT('Ctrl Pts',(-0.100339039978837,-0.0772600332835736,
0.100879686816973));
#18790=CARTESIAN_POINT('Ctrl Pts',(-0.117142637704978,-0.0554368822612891,
0.0991391354240014));
#18791=CARTESIAN_POINT('Ctrl Pts',(-0.126159269908366,-0.0276178718881664,
0.0973985840310299));
#18792=CARTESIAN_POINT('Ctrl Pts',(-0.126349242904067,8.85860673823967E-5,
0.0956580326380584));
#18793=CARTESIAN_POINT('Ctrl Pts',(-0.126529791093031,9.025049583615E-5,
0.109341967361942));
#18794=CARTESIAN_POINT('Ctrl Pts',(-0.126250700293628,-0.0342644551610371,
0.111508106726639));
#18795=CARTESIAN_POINT('Ctrl Pts',(-0.111690189779818,-0.0688279388928191,
0.113674246091336));
#18796=CARTESIAN_POINT('Ctrl Pts',(-0.0867076257192948,-0.092297473337895,
0.115840385456033));
#18797=CARTESIAN_POINT('Ctrl Pts',(-0.0568751199544048,-0.120323220412367,
0.118427044092366));
#18798=CARTESIAN_POINT('Ctrl Pts',(-0.0121812475994092,-0.132529508630403,
0.121013702728699));
#18799=CARTESIAN_POINT('Ctrl Pts',(0.0277554439013372,-0.123558363290506,
0.123600361365031));
#18800=CARTESIAN_POINT('Ctrl Pts',(0.0676921354020838,-0.114587217950609,
0.126187020001364));
#18801=CARTESIAN_POINT('Ctrl Pts',(0.102871646048582,-0.0844386390527785,
0.128773678637697));
#18802=CARTESIAN_POINT('Ctrl Pts',(0.117851793294146,-0.0463464242807743,
0.131360337274029));
#18803=CARTESIAN_POINT('Ctrl Pts',(0.13283194053971,-0.00825420950877041,
0.133946995910362));
#18804=CARTESIAN_POINT('Ctrl Pts',(0.127612724384341,0.0377816411374068,
0.136533654546694));
#18805=CARTESIAN_POINT('Ctrl Pts',(0.104485135941302,0.0715534408109559,
0.139120313183027));
#18806=CARTESIAN_POINT('Ctrl Pts',(0.0813575474982633,0.105325240484505,
0.14170697181936));
#18807=CARTESIAN_POINT('Ctrl Pts',(0.0403215867675544,0.126832989185426,
0.144293630455692));
#18808=CARTESIAN_POINT('Ctrl Pts',(-0.000609841963000384,0.126635909896556,
0.146880289092025));
#18809=CARTESIAN_POINT('Ctrl Pts',(-0.0415412706935549,0.126438830607686,
0.149466947728358));
#18810=CARTESIAN_POINT('Ctrl Pts',(-0.0823681674239554,0.104536923329025,
0.15205360636469));
#18811=CARTESIAN_POINT('Ctrl Pts',(-0.10516942503222,0.0705438627883669,
0.154640265001023));
#18812=CARTESIAN_POINT('Ctrl Pts',(-0.118984510025511,0.0499477610899654,
0.156207499121329));
#18813=CARTESIAN_POINT('Ctrl Pts',(-0.126182304652747,0.0249129445447297,
0.157774733241635));
#18814=CARTESIAN_POINT('Ctrl Pts',(-0.126296536029262,-6.10717992316628E-5,
0.159341967361942));
#18815=CARTESIAN_POINT('Origin',(0.,0.,0.12));
#18816=CARTESIAN_POINT('',(-0.126625441102054,2.7778768752873E-5,0.209341967361942));
#18817=CARTESIAN_POINT('',(-0.126471935391749,0.000101176582396995,0.195658032638058));
#18818=CARTESIAN_POINT('',(-0.12645,1.54856587752183E-17,0.12));
#18819=CARTESIAN_POINT('',(0.0958116152722397,0.0825211298936481,0.24));
#18820=CARTESIAN_POINT('Ctrl Pts',(-0.126625441102054,2.7778768752873E-5,
0.209341967361942));
#18821=CARTESIAN_POINT('Ctrl Pts',(-0.126482885932031,-0.0388928622545336,
0.21180133566563));
#18822=CARTESIAN_POINT('Ctrl Pts',(-0.107125339127294,-0.077921419747323,
0.214260703969318));
#18823=CARTESIAN_POINT('Ctrl Pts',(-0.0759952538809665,-0.101287130411732,
0.216720072273006));
#18824=CARTESIAN_POINT('Ctrl Pts',(-0.0432539585932993,-0.12586218783339,
0.219306730909339));
#18825=CARTESIAN_POINT('Ctrl Pts',(0.0025100419330305,-0.133111106253138,
0.221893389545672));
#18826=CARTESIAN_POINT('Ctrl Pts',(0.0412155518054008,-0.119764891216682,
0.224480048182004));
#18827=CARTESIAN_POINT('Ctrl Pts',(0.0799210616777711,-0.106418676180227,
0.227066706818337));
#18828=CARTESIAN_POINT('Ctrl Pts',(0.111568080896182,-0.072477327687567,
0.229653365454669));
#18829=CARTESIAN_POINT('Ctrl Pts',(0.122246574267713,-0.0330282462555153,
0.232240024091002));
#18830=CARTESIAN_POINT('Ctrl Pts',(0.132925067639245,0.00642083517653631,
0.234826682727335));
#18831=CARTESIAN_POINT('Ctrl Pts',(0.122635035163896,0.0513776495479799,
0.237413341363667));
#18832=CARTESIAN_POINT('Ctrl Pts',(0.0958116152722397,0.0825211298936481,
0.24));
#18833=CARTESIAN_POINT('',(-0.0959791030802601,0.0826138105732953,0.24));
#18834=CARTESIAN_POINT('Origin',(0.,0.,0.24));
#18835=CARTESIAN_POINT('Ctrl Pts',(-0.0959791030802601,0.0826138105732953,
0.24));
#18836=CARTESIAN_POINT('Ctrl Pts',(-0.0710417758635208,0.111296717646776,
0.237599759089979));
#18837=CARTESIAN_POINT('Ctrl Pts',(-0.0322351762885183,0.128218895525122,
0.235199518179958));
#18838=CARTESIAN_POINT('Ctrl Pts',(0.00571352152256588,0.126497857083363,
0.232799277269937));
#18839=CARTESIAN_POINT('Ctrl Pts',(0.0466095526337785,0.124643152028446,
0.230212618633605));
#18840=CARTESIAN_POINT('Ctrl Pts',(0.0865092470399708,0.101136876245298,
0.227625959997272));
#18841=CARTESIAN_POINT('Ctrl Pts',(0.107920636628548,0.0662586835305903,
0.225039301360939));
#18842=CARTESIAN_POINT('Ctrl Pts',(0.129332026217125,0.0313804908158828,
0.222452642724607));
#18843=CARTESIAN_POINT('Ctrl Pts',(0.132255110988087,-0.014869618830384,
0.219865984088274));
#18844=CARTESIAN_POINT('Ctrl Pts',(0.115395215428634,-0.0521699181865619,
0.217279325451942));
#18845=CARTESIAN_POINT('Ctrl Pts',(0.0985353198691812,-0.0894702175427398,
0.214692666815609));
#18846=CARTESIAN_POINT('Ctrl Pts',(0.0618924439793129,-0.117820706608829,
0.212106008179276));
#18847=CARTESIAN_POINT('Ctrl Pts',(0.0215571925812854,-0.12478734248304,
0.209519349542944));
#18848=CARTESIAN_POINT('Ctrl Pts',(-0.0187780588167422,-0.13175397835725,
0.206932690906611));
#18849=CARTESIAN_POINT('Ctrl Pts',(-0.0628056857229291,-0.117336761039583,
0.204346032270278));
#18850=CARTESIAN_POINT('Ctrl Pts',(-0.0912027768750998,-0.0878586653637446,
0.201759373633946));
#18851=CARTESIAN_POINT('Ctrl Pts',(-0.113530209130371,-0.0646812849521466,
0.199725593301983));
#18852=CARTESIAN_POINT('Ctrl Pts',(-0.126194825294183,-0.0321932513395888,
0.197691812970021));
#18853=CARTESIAN_POINT('Ctrl Pts',(-0.126471935391749,0.000101176582396995,
0.195658032638058));
#18854=CARTESIAN_POINT('Origin',(0.,0.,0.350421172358873));
#18855=CARTESIAN_POINT('',(-0.154453350152392,-8.79343647196378E-5,0.0295788276411275));
#18856=CARTESIAN_POINT('',(-0.15422847552802,0.000108763211052777,0.025421172358873));
#18857=CARTESIAN_POINT('',(-0.1543,-1.01731279388251E-15,0.350421172358873));
#18858=CARTESIAN_POINT('',(0.15408394018464,-0.00816268198427004,0.));
#18859=CARTESIAN_POINT('Ctrl Pts',(-0.15422847552802,0.000108763211052763,
0.025421172358873));
#18860=CARTESIAN_POINT('Ctrl Pts',(-0.154338737393477,0.0139570514561378,
0.0247074241482466));
#18861=CARTESIAN_POINT('Ctrl Pts',(-0.146387882101843,0.0778735560251454,
0.0214070173012875));
#18862=CARTESIAN_POINT('Ctrl Pts',(-0.0581466660421577,0.171532975008042,
0.0155199518179959));
#18863=CARTESIAN_POINT('Ctrl Pts',(0.109502662757235,0.144085240745689,
0.00775997590899784));
#18864=CARTESIAN_POINT('Ctrl Pts',(0.156737212705124,0.0419221657566679,
0.00258665863633264));
#18865=CARTESIAN_POINT('Ctrl Pts',(0.15408394018464,-0.00816268198427004,
0.));
#18866=CARTESIAN_POINT('',(0.129620323775263,-0.0841289546921688,3.62607491890453E-17));
#18867=CARTESIAN_POINT('Origin',(0.,0.,0.));
#18868=CARTESIAN_POINT('Ctrl Pts',(-0.154453350152392,-8.7934364719636E-5,
0.0295788276411275));
#18869=CARTESIAN_POINT('Ctrl Pts',(-0.154150470777978,0.0441115087317509,
0.0272927766101045));
#18870=CARTESIAN_POINT('Ctrl Pts',(-0.111454882743928,0.138841433785012,
0.0224200669427489));
#18871=CARTESIAN_POINT('Ctrl Pts',(0.0476444145610997,0.174632482457551,
0.0149606986390605));
#18872=CARTESIAN_POINT('Ctrl Pts',(0.168251138196633,0.0613688951001999,
0.0073871404563744));
#18873=CARTESIAN_POINT('Ctrl Pts',(0.154676764047789,-0.0451013867871701,
0.00240024091002087));
#18874=CARTESIAN_POINT('Ctrl Pts',(0.129620323775263,-0.0841289546921688,
1.57209315010398E-17));
#18875=CARTESIAN_POINT('Origin',(0.,0.,0.350421172358873));
#18876=CARTESIAN_POINT('',(-0.154177051641736,0.000108096719625833,0.0795788276411275));
#18877=CARTESIAN_POINT('',(-0.154234284709463,-0.000121519309271207,0.075421172358873));
#18878=CARTESIAN_POINT('',(-0.1543,-1.01731279388251E-15,0.350421172358873));
#18879=CARTESIAN_POINT('Ctrl Pts',(-0.154234284709463,-0.000121519309271208,
0.0754211723588731));
#18880=CARTESIAN_POINT('Ctrl Pts',(-0.153947235272697,0.0359820467524117,
0.0735607092995758));
#18881=CARTESIAN_POINT('Ctrl Pts',(-0.123557126730793,0.122717061869437,
0.0691135876039459));
#18882=CARTESIAN_POINT('Ctrl Pts',(0.0191012565771036,0.180005302104073,
0.0620798072719832));
#18883=CARTESIAN_POINT('Ctrl Pts',(0.159724738700703,0.0851738948996701,
0.0543198313629854));
#18884=CARTESIAN_POINT('Ctrl Pts',(0.160113920417758,-0.0844204212478698,
0.0465598554539874));
#18885=CARTESIAN_POINT('Ctrl Pts',(0.0199582426985643,-0.179924098035372,
0.0387998795449896));
#18886=CARTESIAN_POINT('Ctrl Pts',(-0.123251388539896,-0.123176028715441,
0.0317536518466181));
#18887=CARTESIAN_POINT('Ctrl Pts',(-0.153939142967466,-0.0362298265692857,
0.0272940827845792));
#18888=CARTESIAN_POINT('Ctrl Pts',(-0.15422847552802,0.000108763211052763,
0.025421172358873));
#18889=CARTESIAN_POINT('Ctrl Pts',(-0.154177051641736,0.000108096719625859,
0.0795788276411275));
#18890=CARTESIAN_POINT('Ctrl Pts',(-0.154289739603949,0.0165429814548096,
0.0787327203977663));
#18891=CARTESIAN_POINT('Ctrl Pts',(-0.144420757340354,0.0830897487115299,
0.0752999545180725));
#18892=CARTESIAN_POINT('Ctrl Pts',(-0.0494457976037486,0.174130301808973,
0.0692805300020459));
#18893=CARTESIAN_POINT('Ctrl Pts',(0.11640175885633,0.13862511662766,0.061520554093048));
#18894=CARTESIAN_POINT('Ctrl Pts',(0.18005704388064,-0.0185795878987759,
0.0537605781840501));
#18895=CARTESIAN_POINT('Ctrl Pts',(0.0856431484406112,-0.159474177462153,
0.0460006022750521));
#18896=CARTESIAN_POINT('Ctrl Pts',(-0.0839657292871194,-0.160363143120653,
0.0382406263660544));
#18897=CARTESIAN_POINT('Ctrl Pts',(-0.151599316432495,-0.0616831513139142,
0.0327667014880793));
#18898=CARTESIAN_POINT('Ctrl Pts',(-0.154493177716258,-0.00590000442131094,
0.0298794352464371));
#18899=CARTESIAN_POINT('Ctrl Pts',(-0.154453350152392,-8.7934364719636E-5,
0.0295788276411275));
#18900=CARTESIAN_POINT('Origin',(0.,0.,0.350421172358873));
#18901=CARTESIAN_POINT('',(-0.154304431028624,-0.000124889850439479,0.129578827641127));
#18902=CARTESIAN_POINT('',(-0.154397364694779,0.000110127730384366,0.125421172358873));
#18903=CARTESIAN_POINT('',(-0.1543,-1.01731279388251E-15,0.350421172358873));
#18904=CARTESIAN_POINT('Ctrl Pts',(-0.154397364694779,0.000110127730384357,
0.125421172358873));
#18905=CARTESIAN_POINT('Ctrl Pts',(-0.154463478494948,0.00824841157753406,
0.125000653087238));
#18906=CARTESIAN_POINT('Ctrl Pts',(-0.150239588102603,0.0663774823757793,
0.121993475179269));
#18907=CARTESIAN_POINT('Ctrl Pts',(-0.0766286530280003,0.163994611436961,
0.116399638634969));
#18908=CARTESIAN_POINT('Ctrl Pts',(0.0927599764682439,0.155440618724813,
0.108639662725971));
#18909=CARTESIAN_POINT('Ctrl Pts',(0.180714016146597,0.0104239566588842,
0.100879686816973));
#18910=CARTESIAN_POINT('Ctrl Pts',(0.11001758793024,-0.143743725357685,
0.093119710907975));
#18911=CARTESIAN_POINT('Ctrl Pts',(-0.0572637123892103,-0.171718146500831,
0.0853597349989769));
#18912=CARTESIAN_POINT('Ctrl Pts',(-0.146220320052713,-0.0783754111826042,
0.0794602221492764));
#18913=CARTESIAN_POINT('Ctrl Pts',(-0.154346328875204,-0.0142138442593302,
0.0761473679359084));
#18914=CARTESIAN_POINT('Ctrl Pts',(-0.154234284709463,-0.000121519309271208,
0.0754211723588731));
#18915=CARTESIAN_POINT('Ctrl Pts',(-0.154304431028624,-0.000124889850439474,
0.129578827641127));
#18916=CARTESIAN_POINT('Ctrl Pts',(-0.153974638929265,0.0385022981904757,
0.127586005549095));
#18917=CARTESIAN_POINT('Ctrl Pts',(-0.120018027207353,0.127784966030512,
0.123006524820731));
#18918=CARTESIAN_POINT('Ctrl Pts',(0.0280571680938306,0.178826694862324,
0.115840385456033));
#18919=CARTESIAN_POINT('Ctrl Pts',(0.163771354656592,0.0771047007047774,
0.108080409547035));
#18920=CARTESIAN_POINT('Ctrl Pts',(0.155709331479018,-0.0923080778690166,
0.100320433638038));
#18921=CARTESIAN_POINT('Ctrl Pts',(0.0109489686262093,-0.180682908560435,
0.0925604577290397));
#18922=CARTESIAN_POINT('Ctrl Pts',(-0.126591758993125,-0.118094248159534,
0.0856465890634029));
#18923=CARTESIAN_POINT('Ctrl Pts',(-0.153945238013925,-0.0337005743957639,
0.0813193790340989));
#18924=CARTESIAN_POINT('Ctrl Pts',(-0.154177051641736,0.000108096719625859,
0.0795788276411275));
#18925=CARTESIAN_POINT('Origin',(0.,0.,0.350421172358873));
#18926=CARTESIAN_POINT('',(-0.154326766555531,0.000123460234585843,0.179578827641127));
#18927=CARTESIAN_POINT('',(-0.154112736333057,-7.45225671948511E-5,0.175421172358873));
#18928=CARTESIAN_POINT('',(-0.1543,-1.01731279388251E-15,0.350421172358873));
#18929=CARTESIAN_POINT('Ctrl Pts',(-0.154112736333057,-7.45225671948471E-5,
0.175421172358873));
#18930=CARTESIAN_POINT('Ctrl Pts',(-0.153973346049181,0.0303998999070902,
0.173853938238567));
#18931=CARTESIAN_POINT('Ctrl Pts',(-0.130694151755309,0.111367805862998,
0.169700045481928));
#18932=CARTESIAN_POINT('Ctrl Pts',(-0.000871711368246156,0.181012066871201,
0.162959494088956));
#18933=CARTESIAN_POINT('Ctrl Pts',(0.149350085565286,0.102277888352765,
0.155199518179958));
#18934=CARTESIAN_POINT('Ctrl Pts',(0.168456255263351,-0.0662471829332422,
0.14743954227096));
#18935=CARTESIAN_POINT('Ctrl Pts',(0.0396733728729688,-0.17661315503135,
0.139679566361963));
#18936=CARTESIAN_POINT('Ctrl Pts',(-0.115072782317819,-0.134350623919955,
0.1323401097246));
#18937=CARTESIAN_POINT('Ctrl Pts',(-0.154056805498669,-0.041811035439686,
0.12758731172357));
#18938=CARTESIAN_POINT('Ctrl Pts',(-0.154397364694779,0.000110127730384357,
0.125421172358873));
#18939=CARTESIAN_POINT('Ctrl Pts',(-0.154326766555531,0.000123460234585825,
0.179578827641127));
#18940=CARTESIAN_POINT('Ctrl Pts',(-0.154418689716183,0.0108361910665024,
0.179025949336757));
#18941=CARTESIAN_POINT('Ctrl Pts',(-0.148597337680631,0.071569631208062,
0.175886412396054));
#18942=CARTESIAN_POINT('Ctrl Pts',(-0.0683530255288039,0.167611467503216,
0.170160216819019));
#18943=CARTESIAN_POINT('Ctrl Pts',(0.100397202365132,0.150621028353064,
0.162400240910021));
#18944=CARTESIAN_POINT('Ctrl Pts',(0.18100910679194,0.00139719974911195,
0.154640265001023));
#18945=CARTESIAN_POINT('Ctrl Pts',(0.102711092909207,-0.149052183789333,
0.146880289092025));
#18946=CARTESIAN_POINT('Ctrl Pts',(-0.0657574679958034,-0.168648048308422,
0.139120313183027));
#18947=CARTESIAN_POINT('Ctrl Pts',(-0.148058381688037,-0.0731761882111772,
0.133353159366061));
#18948=CARTESIAN_POINT('Ctrl Pts',(-0.154402705029802,-0.0116353181791797,
0.130172664185428));
#18949=CARTESIAN_POINT('Ctrl Pts',(-0.154304431028624,-0.000124889850439474,
0.129578827641127));
#18950=CARTESIAN_POINT('Origin',(0.,0.,0.350421172358873));
#18951=CARTESIAN_POINT('',(-0.154128406284035,-0.000157308197905263,0.229578827641128));
#18952=CARTESIAN_POINT('',(-0.154514081154978,3.38969080117728E-5,0.225421172358873));
#18953=CARTESIAN_POINT('',(-0.1543,-1.01731279388251E-15,0.350421172358873));
#18954=CARTESIAN_POINT('',(-0.0398513841857245,-0.149064942821851,0.24));
#18955=CARTESIAN_POINT('Ctrl Pts',(-0.0398513841857245,-0.149064942821851,
0.24));
#18956=CARTESIAN_POINT('Ctrl Pts',(-0.0883048112969314,-0.136111285829332,
0.237413341363667));
#18957=CARTESIAN_POINT('Ctrl Pts',(-0.143745772087175,-0.0847488633265083,
0.233939617244043));
#18958=CARTESIAN_POINT('Ctrl Pts',(-0.154234229255939,-0.017399338864059,
0.230465893124419));
#18959=CARTESIAN_POINT('Ctrl Pts',(-0.154128406284035,-0.00015730819790527,
0.229578827641128));
#18960=CARTESIAN_POINT('',(0.0399565498027962,-0.149273502906638,0.24));
#18961=CARTESIAN_POINT('Origin',(0.,0.,0.24));
#18962=CARTESIAN_POINT('Ctrl Pts',(0.0399565498027963,-0.149273502906638,
0.24));
#18963=CARTESIAN_POINT('Ctrl Pts',(-0.00490373130458673,-0.161043406468747,
0.237599759089979));
#18964=CARTESIAN_POINT('Ctrl Pts',(-0.107666111297752,-0.141562671532916,
0.23274014987627));
#18965=CARTESIAN_POINT('Ctrl Pts',(-0.154340128899266,-0.0474588267763927,
0.227880540662561));
#18966=CARTESIAN_POINT('Ctrl Pts',(-0.154514081154978,3.3896908011755E-5,
0.225421172358873));
#18967=CARTESIAN_POINT('Origin',(0.,0.,0.350421172358873));
#18968=CARTESIAN_POINT('Ctrl Pts',(-0.154514081154978,3.3896908011755E-5,
0.225421172358873));
#18969=CARTESIAN_POINT('Ctrl Pts',(-0.154523084458981,0.00249199339844659,
0.225293882026228));
#18970=CARTESIAN_POINT('Ctrl Pts',(-0.153375868586475,0.0548933889046004,
0.222579933057251));
#18971=CARTESIAN_POINT('Ctrl Pts',(-0.0942515706791253,0.154556313135293,
0.217279325451942));
#18972=CARTESIAN_POINT('Ctrl Pts',(0.0750450248431312,0.164716481511431,
0.209519349542944));
#18973=CARTESIAN_POINT('Ctrl Pts',(0.178461260043253,0.0303012077178856,
0.201759373633945));
#18974=CARTESIAN_POINT('Ctrl Pts',(0.125203781387627,-0.130731709675357,
0.193999397724948));
#18975=CARTESIAN_POINT('Ctrl Pts',(-0.0379704533096903,-0.17698585337688,
0.18623942181595));
#18976=CARTESIAN_POINT('Ctrl Pts',(-0.141587477595567,-0.0899051669249145,
0.180046680027258));
#18977=CARTESIAN_POINT('Ctrl Pts',(-0.154203404262525,-0.019896942829432,
0.176440596874899));
#18978=CARTESIAN_POINT('Ctrl Pts',(-0.154112736333057,-7.45225671948471E-5,
0.175421172358873));
#18979=CARTESIAN_POINT('Ctrl Pts',(-0.154128406284035,-0.00015730819790527,
0.229578827641128));
#18980=CARTESIAN_POINT('Ctrl Pts',(-0.153925652370292,0.0328779499839183,
0.227879234488086));
#18981=CARTESIAN_POINT('Ctrl Pts',(-0.127638532780061,0.116591914860373,
0.223592982698713));
#18982=CARTESIAN_POINT('Ctrl Pts',(0.00818767200092134,0.180778621679153,
0.216720072273006));
#18983=CARTESIAN_POINT('Ctrl Pts',(0.154249898498561,0.0947283641859207,
0.208960096364008));
#18984=CARTESIAN_POINT('Ctrl Pts',(0.164950538597243,-0.0745810526211722,
0.201200120455011));
#18985=CARTESIAN_POINT('Ctrl Pts',(0.0308106631569891,-0.178364693496558,
0.193440144546012));
#18986=CARTESIAN_POINT('Ctrl Pts',(-0.118879635670858,-0.129347344159377,
0.186233046941385));
#18987=CARTESIAN_POINT('Ctrl Pts',(-0.153988624301243,-0.0392836590090855,
0.18161260797309));
#18988=CARTESIAN_POINT('Ctrl Pts',(-0.154326766555531,0.000123460234585825,
0.179578827641127));
#18989=CARTESIAN_POINT('Ctrl Pts',(0.0958116152722397,0.0825211298936481,
0.24));
#18990=CARTESIAN_POINT('Ctrl Pts',(0.122635035163896,0.0513776495479799,
0.237413341363667));
#18991=CARTESIAN_POINT('Ctrl Pts',(0.143215100114593,-0.0385359791949074,
0.232240024091002));
#18992=CARTESIAN_POINT('Ctrl Pts',(0.0482740424593604,-0.140360024672886,
0.224480048182004));
#18993=CARTESIAN_POINT('Ctrl Pts',(-0.0890179591196291,-0.118613269413641,
0.216720072273006));
#18994=CARTESIAN_POINT('Ctrl Pts',(-0.148173729266643,0.00709031985706173,
0.208960096364008));
#18995=CARTESIAN_POINT('Ctrl Pts',(-0.0772398646297824,0.126660050524678,
0.20120012045501));
#18996=CARTESIAN_POINT('Ctrl Pts',(0.0614999571705377,0.134986384232796,
0.193440144546013));
#18997=CARTESIAN_POINT('Ctrl Pts',(0.146250332679645,0.0248320655601208,
0.185680168637014));
#18998=CARTESIAN_POINT('Ctrl Pts',(0.102605431992647,-0.107135610424167,
0.177920192728017));
#18999=CARTESIAN_POINT('Ctrl Pts',(-0.0311170694815965,-0.145041225920327,
0.170160216819019));
#19000=CARTESIAN_POINT('Ctrl Pts',(-0.137521919612742,-0.0556176253575994,
0.162400240910021));
#19001=CARTESIAN_POINT('Ctrl Pts',(-0.123195064154356,0.0826350160503635,
0.154640265001023));
#19002=CARTESIAN_POINT('Ctrl Pts',(-0.000714373963154436,0.148340737886347,
0.146880289092025));
#19003=CARTESIAN_POINT('Ctrl Pts',(0.122393508228972,0.0838174917835845,
0.139120313183027));
#19004=CARTESIAN_POINT('Ctrl Pts',(0.138051156695079,-0.0542900601549481,
0.131360337274029));
#19005=CARTESIAN_POINT('Ctrl Pts',(0.032512624755586,-0.14473579684844,
0.123600361365031));
#19006=CARTESIAN_POINT('Ctrl Pts',(-0.101568992309399,-0.108116932194331,
0.115840385456033));
#19007=CARTESIAN_POINT('Ctrl Pts',(-0.146482409833755,0.0234186855983926,
0.108080409547036));
#19008=CARTESIAN_POINT('Ctrl Pts',(-0.0627977522708403,0.13439480632666,
0.100320433638038));
#19009=CARTESIAN_POINT('Ctrl Pts',(0.076017492057093,0.127384745546031,
0.0925604577290397));
#19010=CARTESIAN_POINT('Ctrl Pts',(0.148096483096158,0.00854251017184644,
0.0848004818200417));
#19011=CARTESIAN_POINT('Ctrl Pts',(0.0901602332714121,-0.117799054254564,
0.0770405059110438));
#19012=CARTESIAN_POINT('Ctrl Pts',(-0.0469280390901857,-0.140724300875114,
0.069280530002046));
#19013=CARTESIAN_POINT('Ctrl Pts',(-0.142818485852497,-0.0401058440029853,
0.0615205540930479));
#19014=CARTESIAN_POINT('Ctrl Pts',(-0.113326201176411,0.0957204333280909,
0.0537605781840501));
#19015=CARTESIAN_POINT('Ctrl Pts',(0.0156536221268617,0.147515686656254,
0.0460006022750521));
#19016=CARTESIAN_POINT('Ctrl Pts',(0.130895613795878,0.0698006416724775,
0.0382406263660543));
#19017=CARTESIAN_POINT('Ctrl Pts',(0.13121455111358,-0.0691831643991777,
0.0304806504570563));
#19018=CARTESIAN_POINT('Ctrl Pts',(0.0163559286405278,-0.147449139316739,
0.0227206745480584));
#19019=CARTESIAN_POINT('Ctrl Pts',(-0.112893560070904,-0.0962328986104914,
0.0149606986390606));
#19020=CARTESIAN_POINT('Ctrl Pts',(-0.142972035491037,0.0393992613429074,
0.00720072273006258));
#19021=CARTESIAN_POINT('Ctrl Pts',(-0.0476516261894416,0.140572551456688,
-0.000559253178935252));
#19022=CARTESIAN_POINT('Ctrl Pts',(0.0897382482543901,0.118078928660352,
-0.00831922908793326));
#19023=CARTESIAN_POINT('Ctrl Pts',(0.128447313976429,0.0343555272840613,
-0.0134925463605985));
#19024=CARTESIAN_POINT('Ctrl Pts',(0.126272937371016,-0.00668937872268922,
-0.0160792049969311));
#19025=CARTESIAN_POINT('Ctrl Pts',(0.102845629995666,0.0885794229410663,
0.245359734998977));
#19026=CARTESIAN_POINT('Ctrl Pts',(0.13163829265517,0.0551495423644061,
0.242773076362644));
#19027=CARTESIAN_POINT('Ctrl Pts',(0.153729244145676,-0.0413651001137901,
0.237599759089979));
#19028=CARTESIAN_POINT('Ctrl Pts',(0.0518180837997932,-0.150664563191773,
0.229839783180981));
#19029=CARTESIAN_POINT('Ctrl Pts',(-0.0955532172229155,-0.127321268762976,
0.222079807271983));
#19030=CARTESIAN_POINT('Ctrl Pts',(-0.159051911315084,0.00761085605850937,
0.214319831362985));
#19031=CARTESIAN_POINT('Ctrl Pts',(-0.0829104333128967,0.135958804728216,
0.206559855453988));
#19032=CARTESIAN_POINT('Ctrl Pts',(0.0660149797280689,0.144896416659008,
0.19879987954499));
#19033=CARTESIAN_POINT('Ctrl Pts',(0.156987308467515,0.0266551129460425,
0.191039903635992));
#19034=CARTESIAN_POINT('Ctrl Pts',(0.110138215124307,-0.11500097684123,
0.183279927726994));
#19035=CARTESIAN_POINT('Ctrl Pts',(-0.0334015307576278,-0.155689435072511,
0.175519951817996));
#19036=CARTESIAN_POINT('Ctrl Pts',(-0.147618098500879,-0.0597007962188336,
0.167759975908998));
#19037=CARTESIAN_POINT('Ctrl Pts',(-0.13223943620312,0.0887016700559064,
0.16));
#19038=CARTESIAN_POINT('Ctrl Pts',(-0.000766819764851659,0.159231180881298,
0.152240024091002));
#19039=CARTESIAN_POINT('Ctrl Pts',(0.131379034007743,0.0899709573066447,
0.144480048182004));
#19040=CARTESIAN_POINT('Ctrl Pts',(0.14818618955117,-0.0582757677477129,
0.136720072273006));
#19041=CARTESIAN_POINT('Ctrl Pts',(0.0348995407947136,-0.15536158290941,
0.128960096364009));
#19042=CARTESIAN_POINT('Ctrl Pts',(-0.109025685167754,-0.116054342400242,
0.12120012045501));
#19043=CARTESIAN_POINT('Ctrl Pts',(-0.157236423577976,0.0251379696208395,
0.113440144546013));
#19044=CARTESIAN_POINT('Ctrl Pts',(-0.0674080525232269,0.144261408030094,
0.105680168637014));
#19045=CARTESIAN_POINT('Ctrl Pts',(0.0815983201941432,0.136736703272292,
0.0979201927280168));
#19046=CARTESIAN_POINT('Ctrl Pts',(0.158968994112971,0.00916965900085902,
0.0901602168190187));
#19047=CARTESIAN_POINT('Ctrl Pts',(0.0967793514910216,-0.126447277955604,
0.0824002409100209));
#19048=CARTESIAN_POINT('Ctrl Pts',(-0.0503732635231939,-0.151055582750353,
0.0746402650010229));
#19049=CARTESIAN_POINT('Ctrl Pts',(-0.15330351242688,-0.0430502166284845,
0.066880289092025));
#19050=CARTESIAN_POINT('Ctrl Pts',(-0.121646050135849,0.102747753924341,
0.0591203131830272));
#19051=CARTESIAN_POINT('Ctrl Pts',(0.0168028336102756,0.158345558472194,
0.0513603372740292));
#19052=CARTESIAN_POINT('Ctrl Pts',(0.140505322097486,0.074925059414875,
0.0436003613650313));
#19053=CARTESIAN_POINT('Ctrl Pts',(0.140847674214973,-0.0742622500154084,
0.0358403854560334));
#19054=CARTESIAN_POINT('Ctrl Pts',(0.0175566999932067,-0.158274125556283,
0.0280804095470355));
#19055=CARTESIAN_POINT('Ctrl Pts',(-0.121181646661057,-0.103297841872129,
0.0203204336380376));
#19056=CARTESIAN_POINT('Ctrl Pts',(-0.153468334920127,0.0422917601656304,
0.0125604577290396));
#19057=CARTESIAN_POINT('Ctrl Pts',(-0.0511499728070136,0.150892692640473,
0.00480048182004178));
#19058=CARTESIAN_POINT('Ctrl Pts',(0.0963263864220051,0.126747699355464,
-0.00295949408895622));
#19059=CARTESIAN_POINT('Ctrl Pts',(0.137877280219327,0.0368777401082635,
-0.00813281136162143));
#19060=CARTESIAN_POINT('Ctrl Pts',(0.135543271642224,-0.00718047980988283,
-0.0107194699979541));
#19061=CARTESIAN_POINT('Ctrl Pts',(0.109879644719093,0.0946377159884845,
0.250719469997954));
#19062=CARTESIAN_POINT('Ctrl Pts',(0.140641550146443,0.0589214351808321,
0.248132811361621));
#19063=CARTESIAN_POINT('Ctrl Pts',(0.164243388176759,-0.0441942210326729,
0.242959494088956));
#19064=CARTESIAN_POINT('Ctrl Pts',(0.055362125140226,-0.160969101710661,
0.235199518179958));
#19065=CARTESIAN_POINT('Ctrl Pts',(-0.102088475326202,-0.13602926811231,
0.227439542270961));
#19066=CARTESIAN_POINT('Ctrl Pts',(-0.169930093363525,0.00813139225995705,
0.219679566361962));
#19067=CARTESIAN_POINT('Ctrl Pts',(-0.0885810019960112,0.145257558931755,
0.211919590452965));
#19068=CARTESIAN_POINT('Ctrl Pts',(0.0705300022856002,0.154806449085219,
0.204159614543967));
#19069=CARTESIAN_POINT('Ctrl Pts',(0.167724284255384,0.0284781603319641,
0.196399638634969));
#19070=CARTESIAN_POINT('Ctrl Pts',(0.117670998255967,-0.122866343258294,
0.188639662725971));
#19071=CARTESIAN_POINT('Ctrl Pts',(-0.0356859920336591,-0.166337644224695,
0.180879686816973));
#19072=CARTESIAN_POINT('Ctrl Pts',(-0.157714277389017,-0.0637839670800676,
0.173119710907975));
#19073=CARTESIAN_POINT('Ctrl Pts',(-0.141283808251885,0.0947683240614489,
0.165359734998977));
#19074=CARTESIAN_POINT('Ctrl Pts',(-0.000819265566548849,0.17012162387625,
0.157599759089979));
#19075=CARTESIAN_POINT('Ctrl Pts',(0.140364559786514,0.0961244228297045,
0.149839783180981));
#19076=CARTESIAN_POINT('Ctrl Pts',(0.158321222407261,-0.0622614753404775,
0.142079807271983));
#19077=CARTESIAN_POINT('Ctrl Pts',(0.0372864568338413,-0.16598736897038,
0.134319831362986));
#19078=CARTESIAN_POINT('Ctrl Pts',(-0.116482378026109,-0.123991752606152,
0.126559855453987));
#19079=CARTESIAN_POINT('Ctrl Pts',(-0.167990437322196,0.0268572536432864,
0.11879987954499));
#19080=CARTESIAN_POINT('Ctrl Pts',(-0.0720183527756138,0.154128009733527,
0.111039903635992));
#19081=CARTESIAN_POINT('Ctrl Pts',(0.0871791483311938,0.146088660998552,
0.103279927726994));
#19082=CARTESIAN_POINT('Ctrl Pts',(0.169841505129784,0.00979680782987164,
0.0955199518179957));
#19083=CARTESIAN_POINT('Ctrl Pts',(0.103398469710631,-0.135095501656644,
0.0877599759089979));
#19084=CARTESIAN_POINT('Ctrl Pts',(-0.0538184879562023,-0.161386864625592,
0.08));
#19085=CARTESIAN_POINT('Ctrl Pts',(-0.163788539001263,-0.0459945892539838,
0.0722400240910021));
#19086=CARTESIAN_POINT('Ctrl Pts',(-0.129965899095288,0.10977507452059,
0.0644800481820042));
#19087=CARTESIAN_POINT('Ctrl Pts',(0.0179520450936897,0.169175430288133,
0.0567200722730062));
#19088=CARTESIAN_POINT('Ctrl Pts',(0.150115030399095,0.0800494771572726,
0.0489600963640084));
#19089=CARTESIAN_POINT('Ctrl Pts',(0.150480797316365,-0.0793413356316391,
0.0412001204550104));
#19090=CARTESIAN_POINT('Ctrl Pts',(0.0187574713458855,-0.169099111795828,
0.0334401445460125));
#19091=CARTESIAN_POINT('Ctrl Pts',(-0.129469733251211,-0.110362785133767,
0.0256801686370146));
#19092=CARTESIAN_POINT('Ctrl Pts',(-0.163964634349217,0.0451842589883535,
0.0179201927280167));
#19093=CARTESIAN_POINT('Ctrl Pts',(-0.0546483194245858,0.161212833824257,
0.0101602168190188));
#19094=CARTESIAN_POINT('Ctrl Pts',(0.10291452458962,0.135416470050577,0.00240024091002082));
#19095=CARTESIAN_POINT('Ctrl Pts',(0.147307246462226,0.0393999529324658,
-0.00277307636264439));
#19096=CARTESIAN_POINT('Ctrl Pts',(0.144813605913432,-0.00767158089707644,
-0.00535973499897704));
#19097=CARTESIAN_POINT('Ctrl Pts',(0.116913659442519,0.100696009035903,
0.256079204996931));
#19098=CARTESIAN_POINT('Ctrl Pts',(0.149644807637716,0.0626933279972582,
0.253492546360598));
#19099=CARTESIAN_POINT('Ctrl Pts',(0.174757532207842,-0.0470233419515556,
0.248319229087933));
#19100=CARTESIAN_POINT('Ctrl Pts',(0.0589061664806588,-0.171273640229548,
0.240559253178935));
#19101=CARTESIAN_POINT('Ctrl Pts',(-0.108623733429488,-0.144737267461644,
0.232799277269938));
#19102=CARTESIAN_POINT('Ctrl Pts',(-0.180808275411966,0.00865192846140473,
0.225039301360939));
#19103=CARTESIAN_POINT('Ctrl Pts',(-0.0942515706791253,0.154556313135293,
0.217279325451942));
#19104=CARTESIAN_POINT('Ctrl Pts',(0.0750450248431312,0.164716481511431,
0.209519349542944));
#19105=CARTESIAN_POINT('Ctrl Pts',(0.178461260043253,0.0303012077178856,
0.201759373633945));
#19106=CARTESIAN_POINT('Ctrl Pts',(0.125203781387627,-0.130731709675357,
0.193999397724948));
#19107=CARTESIAN_POINT('Ctrl Pts',(-0.0379704533096903,-0.17698585337688,
0.18623942181595));
#19108=CARTESIAN_POINT('Ctrl Pts',(-0.167810456277154,-0.0678671379413016,
0.178479445906952));
#19109=CARTESIAN_POINT('Ctrl Pts',(-0.150328180300649,0.100834978066992,
0.170719469997954));
#19110=CARTESIAN_POINT('Ctrl Pts',(-0.000871711368246156,0.181012066871201,
0.162959494088956));
#19111=CARTESIAN_POINT('Ctrl Pts',(0.149350085565286,0.102277888352765,
0.155199518179958));
#19112=CARTESIAN_POINT('Ctrl Pts',(0.168456255263351,-0.0662471829332422,
0.14743954227096));
#19113=CARTESIAN_POINT('Ctrl Pts',(0.0396733728729688,-0.17661315503135,
0.139679566361963));
#19114=CARTESIAN_POINT('Ctrl Pts',(-0.123939070884463,-0.131929162812062,
0.131919590452964));
#19115=CARTESIAN_POINT('Ctrl Pts',(-0.178744451066417,0.0285765376657333,
0.124159614543967));
#19116=CARTESIAN_POINT('Ctrl Pts',(-0.0766286530280003,0.163994611436961,
0.116399638634969));
#19117=CARTESIAN_POINT('Ctrl Pts',(0.0927599764682439,0.155440618724813,
0.108639662725971));
#19118=CARTESIAN_POINT('Ctrl Pts',(0.180714016146597,0.0104239566588842,
0.100879686816973));
#19119=CARTESIAN_POINT('Ctrl Pts',(0.11001758793024,-0.143743725357685,
0.093119710907975));
#19120=CARTESIAN_POINT('Ctrl Pts',(-0.0572637123892103,-0.171718146500831,
0.0853597349989769));
#19121=CARTESIAN_POINT('Ctrl Pts',(-0.174273565575645,-0.048938961879483,
0.0775997590899791));
#19122=CARTESIAN_POINT('Ctrl Pts',(-0.138285748054726,0.11680239511684,
0.0698397831809812));
#19123=CARTESIAN_POINT('Ctrl Pts',(0.0191012565771036,0.180005302104073,
0.0620798072719832));
#19124=CARTESIAN_POINT('Ctrl Pts',(0.159724738700703,0.0851738948996701,
0.0543198313629854));
#19125=CARTESIAN_POINT('Ctrl Pts',(0.160113920417758,-0.0844204212478698,
0.0465598554539874));
#19126=CARTESIAN_POINT('Ctrl Pts',(0.0199582426985643,-0.179924098035372,
0.0387998795449896));
#19127=CARTESIAN_POINT('Ctrl Pts',(-0.137757819841364,-0.117427728395404,
0.0310399036359917));
#19128=CARTESIAN_POINT('Ctrl Pts',(-0.174460933778308,0.0480767578110765,
0.0232799277269937));
#19129=CARTESIAN_POINT('Ctrl Pts',(-0.0581466660421577,0.171532975008042,
0.0155199518179959));
#19130=CARTESIAN_POINT('Ctrl Pts',(0.109502662757235,0.144085240745689,
0.00775997590899784));
#19131=CARTESIAN_POINT('Ctrl Pts',(0.156737212705124,0.0419221657566679,
0.00258665863633264));
#19132=CARTESIAN_POINT('Ctrl Pts',(0.15408394018464,-0.00816268198427004,
0.));
#19133=CARTESIAN_POINT('Ctrl Pts',(0.15408394018464,-0.00816268198427004,
0.));
#19134=CARTESIAN_POINT('Ctrl Pts',(0.153697863146473,0.00250812953454787,
1.45220469349306E-17));
#19135=CARTESIAN_POINT('Ctrl Pts',(0.152123106309386,0.0130673133993916,
-2.32988231788825E-17));
#19136=CARTESIAN_POINT('Ctrl Pts',(0.149466152202855,0.0233620190894148,
-6.07153216591882E-17));
#19137=CARTESIAN_POINT('Ctrl Pts',(0.14793019248835,0.0293132898222067,
-8.23454409684948E-17));
#19138=CARTESIAN_POINT('Ctrl Pts',(0.146031563681721,0.0351760135160456,
3.17823908273165E-17));
#19139=CARTESIAN_POINT('Ctrl Pts',(0.143784059453749,0.0409171473780902,
6.24500451351651E-17));
#19140=CARTESIAN_POINT('Ctrl Pts',(0.142595904075608,0.0439522291322952,
7.86626679846993E-17));
#19141=CARTESIAN_POINT('Ctrl Pts',(0.141309213132582,0.0469553015723855,
1.03399090950918E-16));
#19142=CARTESIAN_POINT('Ctrl Pts',(0.13992871365498,0.0499144025840292,
1.00613961606655E-16));
#19143=CARTESIAN_POINT('Ctrl Pts',(0.135493978469587,0.0594202586791481,
9.16669744478229E-17));
#19144=CARTESIAN_POINT('Ctrl Pts',(0.130119641392827,0.0684241765595774,
5.76730757846686E-17));
#19145=CARTESIAN_POINT('Ctrl Pts',(0.123887660540245,0.0767683201192124,
1.38777878078145E-16));
#19146=CARTESIAN_POINT('Ctrl Pts',(0.120656388342022,0.0810947453345699,
1.808305895663E-16));
#19147=CARTESIAN_POINT('Ctrl Pts',(0.117193874983239,0.0852432898306738,
1.062697842984E-16));
#19148=CARTESIAN_POINT('Ctrl Pts',(0.11350808038867,0.0891875047540603,
1.14491749414469E-16));
#19149=CARTESIAN_POINT('Ctrl Pts',(0.110158526423333,0.0927719043720516,
1.21963656801269E-16));
#19150=CARTESIAN_POINT('Ctrl Pts',(0.106618991420749,0.0961915975683434,
1.17223950247179E-16));
#19151=CARTESIAN_POINT('Ctrl Pts',(0.102922970874274,0.0994011657423757,
1.02348685082632E-16));
#19152=CARTESIAN_POINT('Ctrl Pts',(0.0973787571548163,0.104215676830788,
8.00350512245867E-17));
#19153=CARTESIAN_POINT('Ctrl Pts',(0.0914754811895955,0.108568278221023,
6.56075743842472E-17));
#19154=CARTESIAN_POINT('Ctrl Pts',(0.0852365492443714,0.11239450959967,
3.29597460435593E-17));
#19155=CARTESIAN_POINT('Ctrl Pts',(0.0787787796913796,0.116354950379705,
-7.26807264206779E-19));
#19156=CARTESIAN_POINT('Ctrl Pts',(0.0719608771003193,0.11975150351845,
7.81983513604452E-17));
#19157=CARTESIAN_POINT('Ctrl Pts',(0.0648645680501024,0.122569786811788,
1.05818132034585E-16));
#19158=CARTESIAN_POINT('Ctrl Pts',(0.0619760396963809,0.123716959397427,
1.17060669392563E-16));
#19159=CARTESIAN_POINT('Ctrl Pts',(0.0590419697559043,0.124767587801255,
-1.70921410850511E-17));
#19160=CARTESIAN_POINT('Ctrl Pts',(0.0560804949635964,0.12571697313192,
-8.67361737988404E-19));
#19161=CARTESIAN_POINT('Ctrl Pts',(0.0481895916857994,0.128246627558523,
4.23638569993146E-17));
#19162=CARTESIAN_POINT('Ctrl Pts',(0.040081547172159,0.13006877931966,2.48189907303608E-17));
#19163=CARTESIAN_POINT('Ctrl Pts',(0.0318655688619291,0.131172622122806,
0.));
#19164=CARTESIAN_POINT('Ctrl Pts',(0.0267717292715239,0.131856995664207,
-1.5387571972871E-17));
#19165=CARTESIAN_POINT('Ctrl Pts',(0.0216363184326117,0.132264755542675,
5.61228976213782E-17));
#19166=CARTESIAN_POINT('Ctrl Pts',(0.0164863123329273,0.132388468809724,
3.03576608295941E-17));
#19167=CARTESIAN_POINT('Ctrl Pts',(0.0120733572364389,0.13249447666326,
8.27985532573229E-18));
#19168=CARTESIAN_POINT('Ctrl Pts',(0.00764667637530932,0.132391154756805,
7.9933444120104E-17));
#19169=CARTESIAN_POINT('Ctrl Pts',(0.00324855819595315,0.132074892239241,
9.62771529167128E-17));
#19170=CARTESIAN_POINT('Ctrl Pts',(-0.00215998367955725,0.131685971569047,
1.16375665467493E-16));
#19171=CARTESIAN_POINT('Ctrl Pts',(-0.00753310453775717,0.130975837616781,
1.12286849362194E-16));
#19172=CARTESIAN_POINT('Ctrl Pts',(-0.0128378223015392,0.129936202211006,
1.27068494615301E-16));
#19173=CARTESIAN_POINT('Ctrl Pts',(-0.0180922709275414,0.128906418710228,
1.41710064449709E-16));
#19174=CARTESIAN_POINT('Ctrl Pts',(-0.023283936630727,0.12755123862641,
1.19281234835921E-16));
#19175=CARTESIAN_POINT('Ctrl Pts',(-0.028350637156304,0.125868914531291,
9.19403442267708E-17));
#19176=CARTESIAN_POINT('Ctrl Pts',(-0.0326437071621008,0.124443463179602,
6.87741127091605E-17));
#19177=CARTESIAN_POINT('Ctrl Pts',(-0.0368509055758185,0.122782751372096,
3.08039683582783E-17));
#19178=CARTESIAN_POINT('Ctrl Pts',(-0.0409513668396969,0.120880349084932,
-1.95156391047391E-18));
#19179=CARTESIAN_POINT('Ctrl Pts',(-0.0436523616789034,0.119627226953286,
-2.45035827619675E-17));
#19180=CARTESIAN_POINT('Ctrl Pts',(-0.0463070048384274,0.118269169850402,
-4.56986185075063E-18));
#19181=CARTESIAN_POINT('Ctrl Pts',(-0.0489111879062984,0.116810626195002,
-1.73472347597681E-18));
#19182=CARTESIAN_POINT('Ctrl Pts',(0.0958116152722397,0.0825211298936481,
0.24));
#19183=CARTESIAN_POINT('Ctrl Pts',(0.102494250906434,0.0762804363331629,
0.24));
#19184=CARTESIAN_POINT('Ctrl Pts',(0.108399952301676,0.0693089192431419,
0.24));
#19185=CARTESIAN_POINT('Ctrl Pts',(0.113520383394708,0.0617855200816623,
0.24));
#19186=CARTESIAN_POINT('Ctrl Pts',(0.11760088593285,0.0557900777417299,
0.24));
#19187=CARTESIAN_POINT('Ctrl Pts',(0.1211824537664,0.0494427873910869,0.24));
#19188=CARTESIAN_POINT('Ctrl Pts',(0.124247292533427,0.0428169095598754,
0.24));
#19189=CARTESIAN_POINT('Ctrl Pts',(0.125635784531567,0.0398151273949318,
0.24));
#19190=CARTESIAN_POINT('Ctrl Pts',(0.126914357096627,0.0367636074968772,
0.24));
#19191=CARTESIAN_POINT('Ctrl Pts',(0.128080244072735,0.0336751552254939,
0.24));
#19192=CARTESIAN_POINT('Ctrl Pts',(0.13155694143068,0.024465331227027,0.24));
#19193=CARTESIAN_POINT('Ctrl Pts',(0.134041462136676,0.0149150332268467,
0.24));
#19194=CARTESIAN_POINT('Ctrl Pts',(0.135496608205084,0.00520422800883078,
0.24));
#19195=CARTESIAN_POINT('Ctrl Pts',(0.136052940597398,0.00149158663520877,
0.24));
#19196=CARTESIAN_POINT('Ctrl Pts',(0.136458356591543,-0.00224482315054724,
0.24));
#19197=CARTESIAN_POINT('Ctrl Pts',(0.136708928272429,-0.00599574054845843,
0.24));
#19198=CARTESIAN_POINT('Ctrl Pts',(0.136894600108428,-0.00877514370161729,
0.24));
#19199=CARTESIAN_POINT('Ctrl Pts',(0.136994942037659,-0.0115613689854128,
0.24));
#19200=CARTESIAN_POINT('Ctrl Pts',(0.137008733057845,-0.0143405417274864,
0.24));
#19201=CARTESIAN_POINT('Ctrl Pts',(0.137045731231951,-0.0217964308202384,
0.24));
#19202=CARTESIAN_POINT('Ctrl Pts',(0.136462408227525,-0.0292204075226799,
0.24));
#19203=CARTESIAN_POINT('Ctrl Pts',(0.135240454646173,-0.0365388974416549,
0.24));
#19204=CARTESIAN_POINT('Ctrl Pts',(0.134058793448489,-0.0436160693529878,
0.24));
#19205=CARTESIAN_POINT('Ctrl Pts',(0.132280018312676,-0.050595007513092,
0.24));
#19206=CARTESIAN_POINT('Ctrl Pts',(0.129952822193542,-0.0574290655609092,
0.24));
#19207=CARTESIAN_POINT('Ctrl Pts',(0.128850070284018,-0.0606674134165377,
0.24));
#19208=CARTESIAN_POINT('Ctrl Pts',(0.127623182384127,-0.0638741644409745,
0.24));
#19209=CARTESIAN_POINT('Ctrl Pts',(0.126284110088584,-0.067028198101918,
0.24));
#19210=CARTESIAN_POINT('Ctrl Pts',(0.122654675969015,-0.0755769205431157,
0.24));
#19211=CARTESIAN_POINT('Ctrl Pts',(0.118195290975453,-0.0837663478860722,
0.24));
#19212=CARTESIAN_POINT('Ctrl Pts',(0.113014989178579,-0.0915013065162071,
0.24));
#19213=CARTESIAN_POINT('Ctrl Pts',(0.108985931714537,-0.0975172866704144,
0.24));
#19214=CARTESIAN_POINT('Ctrl Pts',(0.104519884911976,-0.103258562704539,
0.24));
#19215=CARTESIAN_POINT('Ctrl Pts',(0.0996546828651377,-0.108675969178894,
0.24));
#19216=CARTESIAN_POINT('Ctrl Pts',(0.0972822643803542,-0.11131765910988,
0.24));
#19217=CARTESIAN_POINT('Ctrl Pts',(0.09482095240722,-0.113875293456495,
0.24));
#19218=CARTESIAN_POINT('Ctrl Pts',(0.0922773332174137,-0.116342466058553,
0.24));
#19219=CARTESIAN_POINT('Ctrl Pts',(0.0868426048671788,-0.121613857680014,
0.24));
#19220=CARTESIAN_POINT('Ctrl Pts',(0.0810310485854155,-0.126474759557936,
0.24));
#19221=CARTESIAN_POINT('Ctrl Pts',(0.0748870600798396,-0.130870957562724,
0.24));
#19222=CARTESIAN_POINT('Ctrl Pts',(0.0715378781224404,-0.133267392228159,
0.24));
#19223=CARTESIAN_POINT('Ctrl Pts',(0.0680912231566627,-0.135524142754832,
0.24));
#19224=CARTESIAN_POINT('Ctrl Pts',(0.0645638484115253,-0.13762659390894,
0.24));
#19225=CARTESIAN_POINT('Ctrl Pts',(0.0598451535113139,-0.140439117742,0.24));
#19226=CARTESIAN_POINT('Ctrl Pts',(0.0549775790306604,-0.142978967531553,
0.24));
#19227=CARTESIAN_POINT('Ctrl Pts',(0.0499773507040556,-0.145225083935062,
0.24));
#19228=CARTESIAN_POINT('Ctrl Pts',(0.0466920976074369,-0.146700828718701,
0.24));
#19229=CARTESIAN_POINT('Ctrl Pts',(0.0433495270099635,-0.148049731670784,
0.24));
#19230=CARTESIAN_POINT('Ctrl Pts',(0.039956549802796,-0.149273502906639,
0.24));
#19231=CARTESIAN_POINT('Ctrl Pts',(-0.126296536029262,-6.10717992316628E-5,
0.159341967361942));
#19232=CARTESIAN_POINT('Ctrl Pts',(-0.12637083907321,-0.0163056929409037,
0.160361391877968));
#19233=CARTESIAN_POINT('Ctrl Pts',(-0.12344809088261,-0.0325245895549842,
0.161380816393994));
#19234=CARTESIAN_POINT('Ctrl Pts',(-0.117399968681154,-0.0474794518833934,
0.162400240910021));
#19235=CARTESIAN_POINT('Ctrl Pts',(-0.102053636235694,-0.0854254922118417,
0.164986899546353));
#19236=CARTESIAN_POINT('Ctrl Pts',(-0.0665853528586453,-0.115233359066084,
0.167573558182686));
#19237=CARTESIAN_POINT('Ctrl Pts',(-0.0265641275910804,-0.123819689910512,
0.170160216819019));
#19238=CARTESIAN_POINT('Ctrl Pts',(0.0134570976764845,-0.13240602075494,
0.172746875455351));
#19239=CARTESIAN_POINT('Ctrl Pts',(0.058031264834566,-0.119770815589554,
0.175333534091684));
#19240=CARTESIAN_POINT('Ctrl Pts',(0.0875924985281064,-0.0914586003428122,
0.177920192728017));
#19241=CARTESIAN_POINT('Ctrl Pts',(0.117153732221647,-0.0631463850960709,
0.180506851364349));
#19242=CARTESIAN_POINT('Ctrl Pts',(0.131702032450646,-0.0191571597679751,
0.183093510000682));
#19243=CARTESIAN_POINT('Ctrl Pts',(0.124851119980295,0.0211965060081854,
0.185680168637015));
#19244=CARTESIAN_POINT('Ctrl Pts',(0.118000207509943,0.0615501717843459,
0.188266827273347));
#19245=CARTESIAN_POINT('Ctrl Pts',(0.0897500823402403,0.0982682780085711,
0.19085348590968));
#19246=CARTESIAN_POINT('Ctrl Pts',(0.0525017161220023,0.115239608835997,
0.193440144546013));
#19247=CARTESIAN_POINT('Ctrl Pts',(0.0152533499037644,0.132210939663423,
0.196026803182345));
#19248=CARTESIAN_POINT('Ctrl Pts',(-0.030993257363009,0.129435495094051,
0.198613461818678));
#19249=CARTESIAN_POINT('Ctrl Pts',(-0.0659388717692058,0.108119484364762,
0.20120012045501));
#19250=CARTESIAN_POINT('Ctrl Pts',(-0.100884486175403,0.0868034736354726,
0.203786779091343));
#19251=CARTESIAN_POINT('Ctrl Pts',(-0.124529107721023,0.0469468967462671,
0.206373437727676));
#19252=CARTESIAN_POINT('Ctrl Pts',(-0.126492123469331,0.00606801008988057,
0.208960096364008));
#19253=CARTESIAN_POINT('Ctrl Pts',(-0.126588724127832,0.00405634646811867,
0.209087386696653));
#19254=CARTESIAN_POINT('Ctrl Pts',(-0.126632819376787,0.00204220716288977,
0.209214677029297));
#19255=CARTESIAN_POINT('Ctrl Pts',(-0.126625441102054,2.7778768752873E-5,
0.209341967361942));
#19256=CARTESIAN_POINT('Ctrl Pts',(-0.0398513841857245,-0.149064942821851,
0.24));
#19257=CARTESIAN_POINT('Ctrl Pts',(-0.0883048112969314,-0.136111285829332,
0.237413341363667));
#19258=CARTESIAN_POINT('Ctrl Pts',(-0.170871437255804,-0.0596187094618861,
0.232240024091002));
#19259=CARTESIAN_POINT('Ctrl Pts',(-0.145169204726118,0.108307533342445,
0.224480048182004));
#19260=CARTESIAN_POINT('Ctrl Pts',(0.00818767200092134,0.180778621679153,
0.216720072273006));
#19261=CARTESIAN_POINT('Ctrl Pts',(0.154249898498561,0.0947283641859207,
0.208960096364008));
#19262=CARTESIAN_POINT('Ctrl Pts',(0.164950538597243,-0.0745810526211722,
0.201200120455011));
#19263=CARTESIAN_POINT('Ctrl Pts',(0.0308106631569891,-0.178364693496558,
0.193440144546012));
#19264=CARTESIAN_POINT('Ctrl Pts',(-0.13036283225522,-0.125587074703769,
0.185680168637015));
#19265=CARTESIAN_POINT('Ctrl Pts',(-0.17709781441264,0.03745832727601,0.177920192728017));
#19266=CARTESIAN_POINT('Ctrl Pts',(-0.0683530255288039,0.167611467503216,
0.170160216819019));
#19267=CARTESIAN_POINT('Ctrl Pts',(0.100397202365132,0.150621028353064,
0.162400240910021));
#19268=CARTESIAN_POINT('Ctrl Pts',(0.18100910679194,0.00139719974911195,
0.154640265001023));
#19269=CARTESIAN_POINT('Ctrl Pts',(0.102711092909207,-0.149052183789333,
0.146880289092025));
#19270=CARTESIAN_POINT('Ctrl Pts',(-0.0657574679958034,-0.168648048308422,
0.139120313183027));
#19271=CARTESIAN_POINT('Ctrl Pts',(-0.176497206835689,-0.0401861834345609,
0.131360337274029));
#19272=CARTESIAN_POINT('Ctrl Pts',(-0.132288575936487,0.123555290563421,
0.123600361365031));
#19273=CARTESIAN_POINT('Ctrl Pts',(0.0280571680938306,0.178826694862324,
0.115840385456033));
#19274=CARTESIAN_POINT('Ctrl Pts',(0.163771354656592,0.0771047007047774,
0.108080409547035));
#19275=CARTESIAN_POINT('Ctrl Pts',(0.155709331479018,-0.0923080778690166,
0.100320433638038));
#19276=CARTESIAN_POINT('Ctrl Pts',(0.0109489686262093,-0.180682908560435,
0.0925604577290397));
#19277=CARTESIAN_POINT('Ctrl Pts',(-0.143423754439364,-0.110434756566834,
0.0848004818200417));
#19278=CARTESIAN_POINT('Ctrl Pts',(-0.17188331593326,0.0567648465404429,
0.0770405059110439));
#19279=CARTESIAN_POINT('Ctrl Pts',(-0.0494457976037486,0.174130301808973,
0.0692805300020459));
#19280=CARTESIAN_POINT('Ctrl Pts',(0.11640175885633,0.13862511662766,0.061520554093048));
#19281=CARTESIAN_POINT('Ctrl Pts',(0.18005704388064,-0.0185795878987759,
0.0537605781840501));
#19282=CARTESIAN_POINT('Ctrl Pts',(0.0856431484406112,-0.159474177462153,
0.0460006022750521));
#19283=CARTESIAN_POINT('Ctrl Pts',(-0.0839657292871194,-0.160363143120653,
0.0382406263660544));
#19284=CARTESIAN_POINT('Ctrl Pts',(-0.179844832231877,-0.0204718628801216,
0.0304806504570563));
#19285=CARTESIAN_POINT('Ctrl Pts',(-0.117866479118068,0.137399078213474,
0.0227206745480585));
#19286=CARTESIAN_POINT('Ctrl Pts',(0.0476444145610997,0.174632482457551,
0.0149606986390605));
#19287=CARTESIAN_POINT('Ctrl Pts',(0.171219786572432,0.0585809927800803,
0.00720072273006264));
#19288=CARTESIAN_POINT('Ctrl Pts',(0.144688050375066,-0.108949473877577,
-0.000559253178935319));
#19289=CARTESIAN_POINT('Ctrl Pts',(-0.0092814439579932,-0.180735423716049,
-0.00831922908793317));
#19290=CARTESIAN_POINT('Ctrl Pts',(-0.105867686800049,-0.122947365648507,
-0.0134925463605985));
#19291=CARTESIAN_POINT('Ctrl Pts',(-0.131895903200816,-0.0800747195988904,
-0.0160792049969312));
#19292=CARTESIAN_POINT('Ctrl Pts',(-0.0374537582415196,-0.140096572423086,
0.245359734998977));
#19293=CARTESIAN_POINT('Ctrl Pts',(-0.0829920245295529,-0.127922261611689,
0.242773076362644));
#19294=CARTESIAN_POINT('Ctrl Pts',(-0.160591096949962,-0.0560317985556137,
0.237599759089979));
#19295=CARTESIAN_POINT('Ctrl Pts',(-0.13643521822445,0.101791299158848,
0.229839783180981));
#19296=CARTESIAN_POINT('Ctrl Pts',(0.00769506740980954,0.1699022237233,
0.222079807271983));
#19297=CARTESIAN_POINT('Ctrl Pts',(0.144969579481095,0.0890291096113304,
0.214319831362985));
#19298=CARTESIAN_POINT('Ctrl Pts',(0.155026424317845,-0.0700939445729984,
0.206559855453987));
#19299=CARTESIAN_POINT('Ctrl Pts',(0.0289569648011409,-0.167633527556011,
0.19879987954499));
#19300=CARTESIAN_POINT('Ctrl Pts',(-0.122519659046519,-0.118031231043151,
0.191039903635991));
#19301=CARTESIAN_POINT('Ctrl Pts',(-0.166442869216287,0.0352046776440443,
0.183279927726994));
#19302=CARTESIAN_POINT('Ctrl Pts',(-0.064240621638164,0.157527260611955,
0.175519951817996));
#19303=CARTESIAN_POINT('Ctrl Pts',(0.0943568867767351,0.141559037340679,
0.167759975908998));
#19304=CARTESIAN_POINT('Ctrl Pts',(0.170118841887737,0.00131313836865665,
0.16));
#19305=CARTESIAN_POINT('Ctrl Pts',(0.0965315639882279,-0.140084581027326,
0.152240024091002));
#19306=CARTESIAN_POINT('Ctrl Pts',(-0.0618012237018238,-0.158501476380598,
0.144480048182004));
#19307=CARTESIAN_POINT('Ctrl Pts',(-0.165878396703103,-0.0377684145673052,
0.136720072273006));
#19308=CARTESIAN_POINT('Ctrl Pts',(-0.124329541933827,0.116121687534276,
0.128960096364008));
#19309=CARTESIAN_POINT('Ctrl Pts',(0.0263691315170036,0.168067732987372,
0.12120012045501));
#19310=CARTESIAN_POINT('Ctrl Pts',(0.153918185014798,0.0724657594331675,
0.113440144546012));
#19311=CARTESIAN_POINT('Ctrl Pts',(0.146341206869619,-0.0867544378416841,
0.105680168637015));
#19312=CARTESIAN_POINT('Ctrl Pts',(0.0102902328814698,-0.169812269106107,
0.0979201927280167));
#19313=CARTESIAN_POINT('Ctrl Pts',(-0.134794781526993,-0.103790539737311,
0.0901602168190187));
#19314=CARTESIAN_POINT('Ctrl Pts',(-0.161542096774173,0.0533496359633175,
0.0824002409100209));
#19315=CARTESIAN_POINT('Ctrl Pts',(-0.0464709316213242,0.163653894581969,
0.074640265001023));
#19316=CARTESIAN_POINT('Ctrl Pts',(0.109398542213106,0.130284849835523,
0.066880289092025));
#19317=CARTESIAN_POINT('Ctrl Pts',(0.16922405906302,-0.0174617621848401,
0.0591203131830272));
#19318=CARTESIAN_POINT('Ctrl Pts',(0.0804904984426183,-0.149879543972585,
0.0513603372740291));
#19319=CARTESIAN_POINT('Ctrl Pts',(-0.0789139998409189,-0.150715025739123,
0.0436003613650314));
#19320=CARTESIAN_POINT('Ctrl Pts',(-0.169024614954586,-0.0192401899891918,
0.0358403854560333));
#19321=CARTESIAN_POINT('Ctrl Pts',(-0.110775138777956,0.12913257502003,
0.0280804095470356));
#19322=CARTESIAN_POINT('Ctrl Pts',(0.0447779273164969,0.164125861942445,
0.0203204336380375));
#19323=CARTESIAN_POINT('Ctrl Pts',(0.16091848811479,0.0550565152494576,
0.0125604577290397));
#19324=CARTESIAN_POINT('Ctrl Pts',(0.135983012131502,-0.10239461786658,
0.00480048182004171));
#19325=CARTESIAN_POINT('Ctrl Pts',(-0.00872303347143,-0.169861624730324,
-0.00295949408895612));
#19326=CARTESIAN_POINT('Ctrl Pts',(-0.0994982439886826,-0.115550337924785,
-0.00813281136162148));
#19327=CARTESIAN_POINT('Ctrl Pts',(-0.123960494032221,-0.0752570895690155,
-0.0107194699979541));
#19328=CARTESIAN_POINT('Ctrl Pts',(-0.0350561322973148,-0.13112820202432,
0.250719469997954));
#19329=CARTESIAN_POINT('Ctrl Pts',(-0.0776792377621743,-0.119733237394047,
0.248132811361621));
#19330=CARTESIAN_POINT('Ctrl Pts',(-0.150310756644121,-0.0524448876493412,
0.242959494088956));
#19331=CARTESIAN_POINT('Ctrl Pts',(-0.127701231722781,0.0952750649752511,
0.235199518179958));
#19332=CARTESIAN_POINT('Ctrl Pts',(0.00720246281869772,0.159025825767447,
0.22743954227096));
#19333=CARTESIAN_POINT('Ctrl Pts',(0.135689260463629,0.08332985503674,0.219679566361962));
#19334=CARTESIAN_POINT('Ctrl Pts',(0.145102310038447,-0.0656068365248246,
0.211919590452964));
#19335=CARTESIAN_POINT('Ctrl Pts',(0.0271032664452926,-0.156902361615465,
0.204159614543967));
#19336=CARTESIAN_POINT('Ctrl Pts',(-0.114676485837817,-0.110475387382534,
0.196399638634969));
#19337=CARTESIAN_POINT('Ctrl Pts',(-0.155787924019933,0.0329510280120788,
0.188639662725971));
#19338=CARTESIAN_POINT('Ctrl Pts',(-0.0601282177475243,0.147443053720694,
0.180879686816973));
#19339=CARTESIAN_POINT('Ctrl Pts',(0.0883165711883383,0.132497046328295,
0.173119710907975));
#19340=CARTESIAN_POINT('Ctrl Pts',(0.159228576983534,0.00122907698820117,
0.165359734998977));
#19341=CARTESIAN_POINT('Ctrl Pts',(0.0903520350672485,-0.131116978265319,
0.157599759089979));
#19342=CARTESIAN_POINT('Ctrl Pts',(-0.0578449794078444,-0.148354904452775,
0.149839783180981));
#19343=CARTESIAN_POINT('Ctrl Pts',(-0.155259586570517,-0.0353506457000499,
0.142079807271983));
#19344=CARTESIAN_POINT('Ctrl Pts',(-0.116370507931168,0.108688084505131,
0.134319831362985));
#19345=CARTESIAN_POINT('Ctrl Pts',(0.0246810949401768,0.157308771112418,
0.126559855453988));
#19346=CARTESIAN_POINT('Ctrl Pts',(0.144065015373005,0.0678268181615582,
0.118799879544989));
#19347=CARTESIAN_POINT('Ctrl Pts',(0.13697308226022,-0.0812007978143519,
0.111039903635992));
#19348=CARTESIAN_POINT('Ctrl Pts',(0.00963149713673027,-0.15894162965178,
0.103279927726994));
#19349=CARTESIAN_POINT('Ctrl Pts',(-0.126165808614623,-0.0971463229077874,
0.0955199518179957));
#19350=CARTESIAN_POINT('Ctrl Pts',(-0.151200877615086,0.0499344253861922,
0.087759975908998));
#19351=CARTESIAN_POINT('Ctrl Pts',(-0.0434960656388994,0.153177487354966,
0.08));
#19352=CARTESIAN_POINT('Ctrl Pts',(0.102395325569881,0.121944583043386,
0.072240024091002));
#19353=CARTESIAN_POINT('Ctrl Pts',(0.158391074245402,-0.0163439364709043,
0.0644800481820042));
#19354=CARTESIAN_POINT('Ctrl Pts',(0.0753378484446251,-0.140284910483017,
0.0567200722730062));
#19355=CARTESIAN_POINT('Ctrl Pts',(-0.0738622703947183,-0.141066908357593,
0.0489600963640083));
#19356=CARTESIAN_POINT('Ctrl Pts',(-0.158204397677296,-0.018008517098262,
0.0412001204550104));
#19357=CARTESIAN_POINT('Ctrl Pts',(-0.103683798437843,0.120866071826586,
0.0334401445460125));
#19358=CARTESIAN_POINT('Ctrl Pts',(0.0419114400718942,0.153619241427338,
0.0256801686370146));
#19359=CARTESIAN_POINT('Ctrl Pts',(0.150617189657149,0.051532037718835,
0.0179201927280167));
#19360=CARTESIAN_POINT('Ctrl Pts',(0.127277973887939,-0.0958397618555833,
0.0101602168190187));
#19361=CARTESIAN_POINT('Ctrl Pts',(-0.00816462298486686,-0.1589878257446,
0.00240024091002091));
#19362=CARTESIAN_POINT('Ctrl Pts',(-0.0931288011773165,-0.108153310201063,
-0.00277307636264444));
#19363=CARTESIAN_POINT('Ctrl Pts',(-0.116025084863626,-0.0704394595391406,
-0.00535973499897709));
#19364=CARTESIAN_POINT('Ctrl Pts',(-0.0326585063531099,-0.122159831625555,
0.256079204996931));
#19365=CARTESIAN_POINT('Ctrl Pts',(-0.0723664509947957,-0.111544213176404,
0.253492546360598));
#19366=CARTESIAN_POINT('Ctrl Pts',(-0.140030416338279,-0.0488579767430688,
0.248319229087933));
#19367=CARTESIAN_POINT('Ctrl Pts',(-0.118967245221113,0.0887588307916541,
0.240559253178936));
#19368=CARTESIAN_POINT('Ctrl Pts',(0.00670985822758596,0.148149427811594,
0.232799277269937));
#19369=CARTESIAN_POINT('Ctrl Pts',(0.126408941446163,0.0776306004621497,
0.225039301360939));
#19370=CARTESIAN_POINT('Ctrl Pts',(0.13517819575905,-0.0611197284766509,
0.217279325451942));
#19371=CARTESIAN_POINT('Ctrl Pts',(0.0252495680894444,-0.146171195674918,
0.209519349542944));
#19372=CARTESIAN_POINT('Ctrl Pts',(-0.106833312629116,-0.102919543721916,
0.201759373633946));
#19373=CARTESIAN_POINT('Ctrl Pts',(-0.14513297882358,0.0306973783801131,
0.193999397724948));
#19374=CARTESIAN_POINT('Ctrl Pts',(-0.0560158138568844,0.137358846829434,
0.18623942181595));
#19375=CARTESIAN_POINT('Ctrl Pts',(0.0822762555999414,0.12343505531591,
0.178479445906952));
#19376=CARTESIAN_POINT('Ctrl Pts',(0.148338312079331,0.00114501560774606,
0.170719469997954));
#19377=CARTESIAN_POINT('Ctrl Pts',(0.0841725061462688,-0.122149375503312,
0.162959494088956));
#19378=CARTESIAN_POINT('Ctrl Pts',(-0.0538887351138648,-0.138208332524951,
0.155199518179959));
#19379=CARTESIAN_POINT('Ctrl Pts',(-0.144640776437932,-0.0329328768327946,
0.14743954227096));
#19380=CARTESIAN_POINT('Ctrl Pts',(-0.108411473928508,0.101254481475986,
0.139679566361963));
#19381=CARTESIAN_POINT('Ctrl Pts',(0.0229930583633497,0.146549809237466,
0.131919590452964));
#19382=CARTESIAN_POINT('Ctrl Pts',(0.134211845731212,0.0631878768899486,
0.124159614543967));
#19383=CARTESIAN_POINT('Ctrl Pts',(0.127604957650822,-0.0756471577870196,
0.116399638634969));
#19384=CARTESIAN_POINT('Ctrl Pts',(0.00897276139199077,-0.148070990197453,
0.108639662725971));
#19385=CARTESIAN_POINT('Ctrl Pts',(-0.117536835702253,-0.0905021060782641,
0.100879686816973));
#19386=CARTESIAN_POINT('Ctrl Pts',(-0.140859658455999,0.0465192148090667,
0.0931197109079749));
#19387=CARTESIAN_POINT('Ctrl Pts',(-0.0405211996564747,0.142701080127962,
0.0853597349989771));
#19388=CARTESIAN_POINT('Ctrl Pts',(0.0953921089266558,0.113604316251249,
0.077599759089979));
#19389=CARTESIAN_POINT('Ctrl Pts',(0.147558089427783,-0.0152261107569683,
0.0698397831809813));
#19390=CARTESIAN_POINT('Ctrl Pts',(0.070185198446632,-0.130690276993449,
0.0620798072719832));
#19391=CARTESIAN_POINT('Ctrl Pts',(-0.0688105409485176,-0.131418790976063,
0.0543198313629854));
#19392=CARTESIAN_POINT('Ctrl Pts',(-0.147384180400005,-0.0167768442073323,
0.0465598554539874));
#19393=CARTESIAN_POINT('Ctrl Pts',(-0.0965924580977301,0.112599568633142,
0.0387998795449896));
#19394=CARTESIAN_POINT('Ctrl Pts',(0.0390449528272914,0.143112620912232,
0.0310399036359916));
#19395=CARTESIAN_POINT('Ctrl Pts',(0.140315891199508,0.0480075601882123,
0.0232799277269937));
#19396=CARTESIAN_POINT('Ctrl Pts',(0.118572935644375,-0.0892849058445864,
0.0155199518179958));
#19397=CARTESIAN_POINT('Ctrl Pts',(-0.00760621249830358,-0.148114026758875,
0.00775997590899793));
#19398=CARTESIAN_POINT('Ctrl Pts',(-0.0867593583659504,-0.100756282477341,
0.00258665863633259));
#19399=CARTESIAN_POINT('Ctrl Pts',(-0.108089675695031,-0.0656218295092657,
-5.55111512312578E-17));
#19400=CARTESIAN_POINT('Ctrl Pts',(-0.108089675695031,-0.0656218295092657,
-5.55111512312578E-17));
#19401=CARTESIAN_POINT('Ctrl Pts',(-0.104219465379748,-0.0739058869203245,
-4.02841154597017E-17));
#19402=CARTESIAN_POINT('Ctrl Pts',(-0.0994141168358061,-0.0816768736924768,
-5.16144647363644E-17));
#19403=CARTESIAN_POINT('Ctrl Pts',(-0.0938412360364922,-0.088871564406415,
-3.81639164714898E-17));
#19404=CARTESIAN_POINT('Ctrl Pts',(-0.0894001862863345,-0.094605040600905,
-2.74451237748006E-17));
#19405=CARTESIAN_POINT('Ctrl Pts',(-0.0844703330957707,-0.0999727304469881,
3.12377098840079E-17));
#19406=CARTESIAN_POINT('Ctrl Pts',(-0.0791158513129458,-0.104935071387697,
-1.21430643318376E-17));
#19407=CARTESIAN_POINT('Ctrl Pts',(-0.0766900604813501,-0.107183206995485,
-3.17962611543325E-17));
#19408=CARTESIAN_POINT('Ctrl Pts',(-0.0741829996358932,-0.109342173006691,
4.83248416902999E-17));
#19409=CARTESIAN_POINT('Ctrl Pts',(-0.0716059924168524,-0.111405381598006,
5.3776427755281E-17));
#19410=CARTESIAN_POINT('Ctrl Pts',(-0.0639212992135713,-0.117557915794061,
7.00331794132204E-17));
#19411=CARTESIAN_POINT('Ctrl Pts',(-0.0556061968393146,-0.12287204611112,
-5.69073736333764E-18));
#19412=CARTESIAN_POINT('Ctrl Pts',(-0.0468203466856493,-0.127256781127915,
5.55111512312578E-17));
#19413=CARTESIAN_POINT('Ctrl Pts',(-0.0434613267337519,-0.12893315986732,
7.89099528597243E-17));
#19414=CARTESIAN_POINT('Ctrl Pts',(-0.0400330653128497,-0.130473352587733,
3.97002991909352E-17));
#19415=CARTESIAN_POINT('Ctrl Pts',(-0.0365431560942257,-0.131870761756357,
6.59194920871187E-17));
#19416=CARTESIAN_POINT('Ctrl Pts',(-0.0339571636773035,-0.13290622981212,
8.5347686277821E-17));
#19417=CARTESIAN_POINT('Ctrl Pts',(-0.0313383144727484,-0.133862652235137,
-2.74403076010104E-17));
#19418=CARTESIAN_POINT('Ctrl Pts',(-0.0286994266230122,-0.134734580282325,
-2.42861286636753E-17));
#19419=CARTESIAN_POINT('Ctrl Pts',(-0.0216199050576346,-0.137073760181214,
-1.58242011095522E-17));
#19420=CARTESIAN_POINT('Ctrl Pts',(-0.0143790427459088,-0.138813119073991,
5.80198461902811E-17));
#19421=CARTESIAN_POINT('Ctrl Pts',(-0.0070411538297537,-0.139912507657099,
6.93889390390723E-17));
#19422=CARTESIAN_POINT('Ctrl Pts',(5.47883476400097E-5,-0.140975646920361,
8.02325614020808E-17));
#19423=CARTESIAN_POINT('Ctrl Pts',(0.00724182591717642,-0.141440539972256,
1.32011341321413E-16));
#19424=CARTESIAN_POINT('Ctrl Pts',(0.0144605478337719,-0.141339082434075,
1.61329283265843E-16));
#19425=CARTESIAN_POINT('Ctrl Pts',(0.0178811722145177,-0.141291006315792,
1.75221724083914E-16));
#19426=CARTESIAN_POINT('Ctrl Pts',(0.021310106848269,-0.141115105569205,
1.85534911235541E-16));
#19427=CARTESIAN_POINT('Ctrl Pts',(0.0247235715439624,-0.140816220288761,
1.71737624121704E-16));
#19428=CARTESIAN_POINT('Ctrl Pts',(0.0339754553361668,-0.140006119078294,
1.34341339582434E-16));
#19429=CARTESIAN_POINT('Ctrl Pts',(0.0431421008898472,-0.138295657968001,
8.04496487960062E-17));
#19430=CARTESIAN_POINT('Ctrl Pts',(0.0520992976556894,-0.135759125106636,
3.20923843055709E-17));
#19431=CARTESIAN_POINT('Ctrl Pts',(0.0590658916121619,-0.13378629867842,
-5.518202506064E-18));
#19432=CARTESIAN_POINT('Ctrl Pts',(0.0659062642374416,-0.131312982137409,
7.87850579480063E-17));
#19433=CARTESIAN_POINT('Ctrl Pts',(0.0725619642951071,-0.128359965266718,
7.63278329429795E-17));
#19434=CARTESIAN_POINT('Ctrl Pts',(0.0758074813473741,-0.126919986522721,
7.51296170399226E-17));
#19435=CARTESIAN_POINT('Ctrl Pts',(0.0790005264283722,-0.125369490597537,
8.38688896655138E-17));
#19436=CARTESIAN_POINT('Ctrl Pts',(0.0821329715644795,-0.123712761836801,
7.24247051220317E-17));
#19437=CARTESIAN_POINT('Ctrl Pts',(0.0888257654942848,-0.120172989003949,
4.79730178566093E-17));
#19438=CARTESIAN_POINT('Ctrl Pts',(0.0952446087626691,-0.116147988031934,
8.96774285244103E-17));
#19439=CARTESIAN_POINT('Ctrl Pts',(0.101324221742587,-0.111663228753314,
8.28330459778925E-17));
#19440=CARTESIAN_POINT('Ctrl Pts',(0.104638321741973,-0.109218510516871,
7.91020571356516E-17));
#19441=CARTESIAN_POINT('Ctrl Pts',(0.107849695272814,-0.106637925639498,
3.17151869302413E-17));
#19442=CARTESIAN_POINT('Ctrl Pts',(0.110939265073957,-0.10393289123317,
1.53956708492942E-17));
#19443=CARTESIAN_POINT('Ctrl Pts',(0.115072333360666,-0.100314234708527,
-6.43574216607592E-18));
#19444=CARTESIAN_POINT('Ctrl Pts',(0.118992075260627,-0.0964697210975667,
5.54296751400654E-17));
#19445=CARTESIAN_POINT('Ctrl Pts',(0.122673447199167,-0.0924082746861152,
3.52365706057789E-17));
#19446=CARTESIAN_POINT('Ctrl Pts',(0.125092164655522,-0.0897398425098966,
2.31620156359627E-17));
#19447=CARTESIAN_POINT('Ctrl Pts',(0.127407959881093,-0.0869777021544565,
-4.01489640485901E-17));
#19448=CARTESIAN_POINT('Ctrl Pts',(0.129620323775263,-0.0841289546921697,
-3.98986399474666E-17));
#19449=CARTESIAN_POINT('Ctrl Pts',(-0.126471935391749,0.000101176582396995,
0.195658032638058));
#19450=CARTESIAN_POINT('Ctrl Pts',(-0.126547267107008,0.00888033934128026,
0.195105154333688));
#19451=CARTESIAN_POINT('Ctrl Pts',(-0.125707148272093,0.0176451944231377,
0.194552276029318));
#19452=CARTESIAN_POINT('Ctrl Pts',(-0.12389684029672,0.0262048027713284,
0.193999397724948));
#19453=CARTESIAN_POINT('Ctrl Pts',(-0.115427257168015,0.0662512011965534,
0.191412739088615));
#19454=CARTESIAN_POINT('Ctrl Pts',(-0.0857215355124495,0.101805024012994,
0.188826080452282));
#19455=CARTESIAN_POINT('Ctrl Pts',(-0.0478199964418627,0.117261303502293,
0.18623942181595));
#19456=CARTESIAN_POINT('Ctrl Pts',(-0.0099184573712758,0.132717582991593,
0.183652763179617));
#19457=CARTESIAN_POINT('Ctrl Pts',(0.0361788991143328,0.128076319153751,
0.181066104543285));
#19458=CARTESIAN_POINT('Ctrl Pts',(0.070237920103702,0.105374013950137,
0.178479445906952));
#19459=CARTESIAN_POINT('Ctrl Pts',(0.104296941093071,0.0826717087465222,
0.175892787270619));
#19460=CARTESIAN_POINT('Ctrl Pts',(0.126317626586201,0.0419083621771342,
0.173306128634287));
#19461=CARTESIAN_POINT('Ctrl Pts',(0.126633668343922,0.000977623707263797,
0.170719469997954));
#19462=CARTESIAN_POINT('Ctrl Pts',(0.126949710101644,-0.0399531147626067,
0.168132811361621));
#19463=CARTESIAN_POINT('Ctrl Pts',(0.105561108123956,-0.08105124513296,
0.165546152725289));
#19464=CARTESIAN_POINT('Ctrl Pts',(0.0718566002584231,-0.104276803155076,
0.162959494088956));
#19465=CARTESIAN_POINT('Ctrl Pts',(0.0381520923928904,-0.127502361177192,
0.160372835452623));
#19466=CARTESIAN_POINT('Ctrl Pts',(-0.00786832136048696,-0.132855346851071,
0.157786176816291));
#19467=CARTESIAN_POINT('Ctrl Pts',(-0.0460038684578537,-0.117985930405985,
0.155199518179958));
#19468=CARTESIAN_POINT('Ctrl Pts',(-0.0841394155552204,-0.103116513960899,
0.152612859543626));
#19469=CARTESIAN_POINT('Ctrl Pts',(-0.114390095996576,-0.0680246953968468,
0.150026200907293));
#19470=CARTESIAN_POINT('Ctrl Pts',(-0.12347721913235,-0.0281142263966907,
0.14743954227096));
#19471=CARTESIAN_POINT('Ctrl Pts',(-0.125563410841138,-0.018951712774069,
0.14684570572666));
#19472=CARTESIAN_POINT('Ctrl Pts',(-0.126534167537385,-0.00953522996602069,
0.146251869182359));
#19473=CARTESIAN_POINT('Ctrl Pts',(-0.126453631260982,-0.000102348163238207,
0.145658032638058));
#19474=CARTESIAN_POINT('Ctrl Pts',(-0.0398513841857245,-0.149064942821851,
0.24));
#19475=CARTESIAN_POINT('Ctrl Pts',(-0.0498806325786677,-0.145400296738327,
0.24));
#19476=CARTESIAN_POINT('Ctrl Pts',(-0.0594363948008725,-0.140639648297949,
0.24));
#19477=CARTESIAN_POINT('Ctrl Pts',(-0.0684062055177017,-0.134931499399492,
0.24));
#19478=CARTESIAN_POINT('Ctrl Pts',(-0.0735915624001909,-0.131631676235849,
0.24));
#19479=CARTESIAN_POINT('Ctrl Pts',(-0.0785806353345173,-0.128014298080738,
0.24));
#19480=CARTESIAN_POINT('Ctrl Pts',(-0.0833462611484583,-0.124102693747304,
0.24));
#19481=CARTESIAN_POINT('Ctrl Pts',(-0.0858656342542594,-0.122034803580736,
0.24));
#19482=CARTESIAN_POINT('Ctrl Pts',(-0.0883241156266364,-0.11988309220465,
0.24));
#19483=CARTESIAN_POINT('Ctrl Pts',(-0.0907117892851122,-0.117655751751618,
0.24));
#19484=CARTESIAN_POINT('Ctrl Pts',(-0.0983819858496404,-0.110500611839494,
0.24));
#19485=CARTESIAN_POINT('Ctrl Pts',(-0.105284458416918,-0.102606966330569,
0.24));
#19486=CARTESIAN_POINT('Ctrl Pts',(-0.111294422020379,-0.0941015332659665,
0.24));
#19487=CARTESIAN_POINT('Ctrl Pts',(-0.114410577497229,-0.0896914812962706,
0.24));
#19488=CARTESIAN_POINT('Ctrl Pts',(-0.117286101138547,-0.0851164738413172,
0.24));
#19489=CARTESIAN_POINT('Ctrl Pts',(-0.119898298320422,-0.0803922539627851,
0.24));
#19490=CARTESIAN_POINT('Ctrl Pts',(-0.1222721977331,-0.0760990011896685,
0.24));
#19491=CARTESIAN_POINT('Ctrl Pts',(-0.124430744329062,-0.0716759619599862,
0.24));
#19492=CARTESIAN_POINT('Ctrl Pts',(-0.126341093034125,-0.0671690272221462,
0.24));
#19493=CARTESIAN_POINT('Ctrl Pts',(-0.129206708925078,-0.060408406100978,
0.24));
#19494=CARTESIAN_POINT('Ctrl Pts',(-0.131522065955468,-0.0534490321795157,
0.24));
#19495=CARTESIAN_POINT('Ctrl Pts',(-0.133233091500091,-0.0463330844490581,
0.24));
#19496=CARTESIAN_POINT('Ctrl Pts',(-0.135004134506116,-0.0389675313754268,
0.24));
#19497=CARTESIAN_POINT('Ctrl Pts',(-0.136127599829873,-0.0314337185245799,
0.24));
#19498=CARTESIAN_POINT('Ctrl Pts',(-0.136615064298196,-0.0238138180582873,
0.24));
#19499=CARTESIAN_POINT('Ctrl Pts',(-0.136813484749433,-0.0207121682209076,
0.24));
#19500=CARTESIAN_POINT('Ctrl Pts',(-0.136906013213758,-0.0175970392000076,
0.24));
#19501=CARTESIAN_POINT('Ctrl Pts',(-0.136893785357156,-0.0144871321155608,
0.24));
#19502=CARTESIAN_POINT('Ctrl Pts',(-0.136861203984761,-0.00620072149302863,
0.24));
#19503=CARTESIAN_POINT('Ctrl Pts',(-0.136088646936857,0.00207357465703332,
0.24));
#19504=CARTESIAN_POINT('Ctrl Pts',(-0.134599584032292,0.0102285531249486,
0.24));
#19505=CARTESIAN_POINT('Ctrl Pts',(-0.133676409755049,0.0152843948425598,
0.24));
#19506=CARTESIAN_POINT('Ctrl Pts',(-0.132477333465274,0.0202942984003417,
0.24));
#19507=CARTESIAN_POINT('Ctrl Pts',(-0.131003622030167,0.0252303138624672,
0.24));
#19508=CARTESIAN_POINT('Ctrl Pts',(-0.129740734874544,0.029460199292259,
0.24));
#19509=CARTESIAN_POINT('Ctrl Pts',(-0.128274507607502,0.0336384499732856,
0.24));
#19510=CARTESIAN_POINT('Ctrl Pts',(-0.126614574688298,0.0377237273426867,
0.24));
#19511=CARTESIAN_POINT('Ctrl Pts',(-0.124573382985647,0.042747324485064,
0.24));
#19512=CARTESIAN_POINT('Ctrl Pts',(-0.122237651925267,0.0476379767326878,
0.24));
#19513=CARTESIAN_POINT('Ctrl Pts',(-0.119609691052418,0.0523617558795304,
0.24));
#19514=CARTESIAN_POINT('Ctrl Pts',(-0.117006563775536,0.0570408964535612,
0.24));
#19515=CARTESIAN_POINT('Ctrl Pts',(-0.114113358229268,0.0615597689541448,
0.24));
#19516=CARTESIAN_POINT('Ctrl Pts',(-0.110947628485839,0.0658586917144141,
0.24));
#19517=CARTESIAN_POINT('Ctrl Pts',(-0.108265305855902,0.0695011687224882,
0.24));
#19518=CARTESIAN_POINT('Ctrl Pts',(-0.105385772272888,0.0729892759232728,
0.24));
#19519=CARTESIAN_POINT('Ctrl Pts',(-0.102309360287629,0.0763011815833395,
0.24));
#19520=CARTESIAN_POINT('Ctrl Pts',(-0.100282916666232,0.0784827457339379,
0.24));
#19521=CARTESIAN_POINT('Ctrl Pts',(-0.0981709975111385,0.0805877996091198,
0.24));
#19522=CARTESIAN_POINT('Ctrl Pts',(-0.0959791030802606,0.0826138105732947,
0.24));
#19523=CARTESIAN_POINT('Origin',(0.,0.,0.24));
#19524=CARTESIAN_POINT('',(0.158771324027147,-0.275,0.24));
#19525=CARTESIAN_POINT('',(0.317542648054294,0.,0.24));
#19526=CARTESIAN_POINT('',(0.158771324027147,-0.275,0.24));
#19527=CARTESIAN_POINT('',(0.158771324027147,0.275,0.24));
#19528=CARTESIAN_POINT('',(0.317542648054294,0.,0.24));
#19529=CARTESIAN_POINT('',(-0.158771324027147,0.275,0.24));
#19530=CARTESIAN_POINT('',(0.158771324027147,0.275,0.24));
#19531=CARTESIAN_POINT('',(-0.317542648054294,5.55111512312578E-17,0.24));
#19532=CARTESIAN_POINT('',(-0.158771324027147,0.275,0.24));
#19533=CARTESIAN_POINT('',(-0.158771324027147,-0.275,0.24));
#19534=CARTESIAN_POINT('',(-0.317542648054294,3.88877587532466E-17,0.24));
#19535=CARTESIAN_POINT('',(-0.158771324027147,-0.275,0.24));
#19536=CARTESIAN_POINT('Origin',(0.,0.,0.12));
#19537=CARTESIAN_POINT('Origin',(-0.158771324027147,-0.275,0.));
#19538=CARTESIAN_POINT('',(-0.158771324027147,-0.275,0.));
#19539=CARTESIAN_POINT('',(0.158771324027147,-0.275,0.));
#19540=CARTESIAN_POINT('',(-0.158771324027147,-0.275,0.));
#19541=CARTESIAN_POINT('',(0.158771324027147,-0.275,0.));
#19542=CARTESIAN_POINT('',(-0.158771324027147,-0.275,0.));
#19543=CARTESIAN_POINT('Origin',(-0.317542648054294,3.88877587532466E-17,
0.));
#19544=CARTESIAN_POINT('',(-0.317542648054294,3.88877587532466E-17,0.));
#19545=CARTESIAN_POINT('',(-0.317542648054294,3.88877587532466E-17,0.));
#19546=CARTESIAN_POINT('',(-0.317542648054294,3.88877587532466E-17,0.));
#19547=CARTESIAN_POINT('Origin',(-0.158771324027147,0.275,0.));
#19548=CARTESIAN_POINT('',(-0.158771324027147,0.275,0.));
#19549=CARTESIAN_POINT('',(-0.158771324027147,0.275,0.));
#19550=CARTESIAN_POINT('',(-0.158771324027147,0.275,0.));
#19551=CARTESIAN_POINT('Origin',(0.158771324027147,0.275,0.));
#19552=CARTESIAN_POINT('',(0.158771324027147,0.275,0.));
#19553=CARTESIAN_POINT('',(0.158771324027147,0.275,0.));
#19554=CARTESIAN_POINT('',(0.158771324027147,0.275,0.));
#19555=CARTESIAN_POINT('Origin',(0.317542648054294,0.,0.));
#19556=CARTESIAN_POINT('',(0.317542648054294,0.,0.));
#19557=CARTESIAN_POINT('',(0.317542648054294,0.,0.));
#19558=CARTESIAN_POINT('',(0.317542648054294,0.,0.));
#19559=CARTESIAN_POINT('Origin',(0.158771324027147,-0.275,0.));
#19560=CARTESIAN_POINT('',(0.158771324027147,-0.275,0.));
#19561=CARTESIAN_POINT('Origin',(0.,0.,0.));
#19562=CARTESIAN_POINT('',(0.,0.,0.));
#19563=CARTESIAN_POINT('',(0.,0.,0.));
#19564=CARTESIAN_POINT('',(0.,0.,0.));
#19565=CARTESIAN_POINT('',(2.,0.,0.6));
#19566=CARTESIAN_POINT('',(2.,0.,-0.84));
#19567=CARTESIAN_POINT('',(0.,0.,0.));
#19568=CARTESIAN_POINT('',(11.2,0.,0.6));
#19569=CARTESIAN_POINT('',(11.2,0.,-0.84));
#19570=CARTESIAN_POINT('',(0.,0.,0.));
#19571=CARTESIAN_POINT('Origin',(0.,0.,0.));
#19572=CARTESIAN_POINT('',(-0.41,-5.02105187650415E-17,0.1));
#19573=CARTESIAN_POINT('Origin',(0.,0.,0.1));
#19574=CARTESIAN_POINT('',(-0.41,-5.02105187650415E-17,0.));
#19575=CARTESIAN_POINT('',(-0.41,-5.02105187650415E-17,0.));
#19576=CARTESIAN_POINT('Origin',(0.,0.,0.));
#19577=CARTESIAN_POINT('Origin',(0.,0.,0.));
#19578=CARTESIAN_POINT('',(-0.6,-7.34788079488412E-17,0.1));
#19579=CARTESIAN_POINT('Origin',(0.,0.,0.1));
#19580=CARTESIAN_POINT('',(-0.6,-7.34788079488412E-17,0.));
#19581=CARTESIAN_POINT('',(-0.6,-7.34788079488412E-17,0.));
#19582=CARTESIAN_POINT('Origin',(0.,0.,0.));
#19583=CARTESIAN_POINT('Origin',(0.,0.,0.1));
#19584=CARTESIAN_POINT('Origin',(0.,0.,0.));
#19585=CARTESIAN_POINT('',(0.,0.,0.));
#19586=CARTESIAN_POINT('',(0.,3.01360886158311E-60,-1.55386011266781E-76));
#19587=CARTESIAN_POINT('',(4.,-2.5,0.3));
#19588=CARTESIAN_POINT('',(0.,0.,0.));
#19589=CARTESIAN_POINT('',(0.,0.,0.6));
#19590=CARTESIAN_POINT('',(0.,0.,0.7));
#19591=CARTESIAN_POINT('',(3.99999999999999,2.5,-0.3));
#19592=CARTESIAN_POINT('',(0.,0.,-0.7));
#19593=UNCERTAINTY_MEASURE_WITH_UNIT(LENGTH_MEASURE(0.001),#19619,
'DISTANCE_ACCURACY_VALUE',
'Maximum model space distance between geometric entities at asserted c
onnectivities');
#19594=UNCERTAINTY_MEASURE_WITH_UNIT(LENGTH_MEASURE(0.001),#19619,
'DISTANCE_ACCURACY_VALUE',
'Maximum model space distance between geometric entities at asserted c
onnectivities');
#19595=UNCERTAINTY_MEASURE_WITH_UNIT(LENGTH_MEASURE(0.001),#19619,
'DISTANCE_ACCURACY_VALUE',
'Maximum model space distance between geometric entities at asserted c
onnectivities');
#19596=UNCERTAINTY_MEASURE_WITH_UNIT(LENGTH_MEASURE(0.001),#19619,
'DISTANCE_ACCURACY_VALUE',
'Maximum model space distance between geometric entities at asserted c
onnectivities');
#19597=UNCERTAINTY_MEASURE_WITH_UNIT(LENGTH_MEASURE(0.001),#19619,
'DISTANCE_ACCURACY_VALUE',
'Maximum model space distance between geometric entities at asserted c
onnectivities');
#19598=UNCERTAINTY_MEASURE_WITH_UNIT(LENGTH_MEASURE(0.001),#19619,
'DISTANCE_ACCURACY_VALUE',
'Maximum model space distance between geometric entities at asserted c
onnectivities');
#19599=UNCERTAINTY_MEASURE_WITH_UNIT(LENGTH_MEASURE(0.001),#19619,
'DISTANCE_ACCURACY_VALUE',
'Maximum model space distance between geometric entities at asserted c
onnectivities');
#19600=UNCERTAINTY_MEASURE_WITH_UNIT(LENGTH_MEASURE(0.001),#19619,
'DISTANCE_ACCURACY_VALUE',
'Maximum model space distance between geometric entities at asserted c
onnectivities');
#19601=UNCERTAINTY_MEASURE_WITH_UNIT(LENGTH_MEASURE(0.001),#19619,
'DISTANCE_ACCURACY_VALUE',
'Maximum model space distance between geometric entities at asserted c
onnectivities');
#19602=UNCERTAINTY_MEASURE_WITH_UNIT(LENGTH_MEASURE(0.001),#19619,
'DISTANCE_ACCURACY_VALUE',
'Maximum model space distance between geometric entities at asserted c
onnectivities');
#19603=UNCERTAINTY_MEASURE_WITH_UNIT(LENGTH_MEASURE(0.001),#19619,
'DISTANCE_ACCURACY_VALUE',
'Maximum model space distance between geometric entities at asserted c
onnectivities');
#19604=UNCERTAINTY_MEASURE_WITH_UNIT(LENGTH_MEASURE(0.001),#19619,
'DISTANCE_ACCURACY_VALUE',
'Maximum model space distance between geometric entities at asserted c
onnectivities');
#19605=UNCERTAINTY_MEASURE_WITH_UNIT(LENGTH_MEASURE(0.001),#19619,
'DISTANCE_ACCURACY_VALUE',
'Maximum model space distance between geometric entities at asserted c
onnectivities');
#19606=(
GEOMETRIC_REPRESENTATION_CONTEXT(3)
GLOBAL_UNCERTAINTY_ASSIGNED_CONTEXT((#19593))
GLOBAL_UNIT_ASSIGNED_CONTEXT((#19619,#19621,#19622))
REPRESENTATION_CONTEXT('','3D')
);
#19607=(
GEOMETRIC_REPRESENTATION_CONTEXT(3)
GLOBAL_UNCERTAINTY_ASSIGNED_CONTEXT((#19594))
GLOBAL_UNIT_ASSIGNED_CONTEXT((#19619,#19621,#19622))
REPRESENTATION_CONTEXT('','3D')
);
#19608=(
GEOMETRIC_REPRESENTATION_CONTEXT(3)
GLOBAL_UNCERTAINTY_ASSIGNED_CONTEXT((#19595))
GLOBAL_UNIT_ASSIGNED_CONTEXT((#19619,#19621,#19622))
REPRESENTATION_CONTEXT('','3D')
);
#19609=(
GEOMETRIC_REPRESENTATION_CONTEXT(3)
GLOBAL_UNCERTAINTY_ASSIGNED_CONTEXT((#19596))
GLOBAL_UNIT_ASSIGNED_CONTEXT((#19619,#19621,#19622))
REPRESENTATION_CONTEXT('','3D')
);
#19610=(
GEOMETRIC_REPRESENTATION_CONTEXT(3)
GLOBAL_UNCERTAINTY_ASSIGNED_CONTEXT((#19597))
GLOBAL_UNIT_ASSIGNED_CONTEXT((#19619,#19621,#19622))
REPRESENTATION_CONTEXT('','3D')
);
#19611=(
GEOMETRIC_REPRESENTATION_CONTEXT(3)
GLOBAL_UNCERTAINTY_ASSIGNED_CONTEXT((#19598))
GLOBAL_UNIT_ASSIGNED_CONTEXT((#19619,#19621,#19622))
REPRESENTATION_CONTEXT('','3D')
);
#19612=(
GEOMETRIC_REPRESENTATION_CONTEXT(3)
GLOBAL_UNCERTAINTY_ASSIGNED_CONTEXT((#19599))
GLOBAL_UNIT_ASSIGNED_CONTEXT((#19619,#19621,#19622))
REPRESENTATION_CONTEXT('','3D')
);
#19613=(
GEOMETRIC_REPRESENTATION_CONTEXT(3)
GLOBAL_UNCERTAINTY_ASSIGNED_CONTEXT((#19600))
GLOBAL_UNIT_ASSIGNED_CONTEXT((#19619,#19621,#19622))
REPRESENTATION_CONTEXT('','3D')
);
#19614=(
GEOMETRIC_REPRESENTATION_CONTEXT(3)
GLOBAL_UNCERTAINTY_ASSIGNED_CONTEXT((#19601))
GLOBAL_UNIT_ASSIGNED_CONTEXT((#19619,#19621,#19622))
REPRESENTATION_CONTEXT('','3D')
);
#19615=(
GEOMETRIC_REPRESENTATION_CONTEXT(3)
GLOBAL_UNCERTAINTY_ASSIGNED_CONTEXT((#19602))
GLOBAL_UNIT_ASSIGNED_CONTEXT((#19619,#19621,#19622))
REPRESENTATION_CONTEXT('','3D')
);
#19616=(
GEOMETRIC_REPRESENTATION_CONTEXT(3)
GLOBAL_UNCERTAINTY_ASSIGNED_CONTEXT((#19603))
GLOBAL_UNIT_ASSIGNED_CONTEXT((#19619,#19621,#19622))
REPRESENTATION_CONTEXT('','3D')
);
#19617=(
GEOMETRIC_REPRESENTATION_CONTEXT(3)
GLOBAL_UNCERTAINTY_ASSIGNED_CONTEXT((#19604))
GLOBAL_UNIT_ASSIGNED_CONTEXT((#19619,#19621,#19622))
REPRESENTATION_CONTEXT('','3D')
);
#19618=(
GEOMETRIC_REPRESENTATION_CONTEXT(3)
GLOBAL_UNCERTAINTY_ASSIGNED_CONTEXT((#19605))
GLOBAL_UNIT_ASSIGNED_CONTEXT((#19619,#19621,#19622))
REPRESENTATION_CONTEXT('','3D')
);
#19619=(
LENGTH_UNIT()
NAMED_UNIT(*)
SI_UNIT(.CENTI.,.METRE.)
);
#19620=(
LENGTH_UNIT()
NAMED_UNIT(*)
SI_UNIT($,.METRE.)
);
#19621=(
NAMED_UNIT(*)
PLANE_ANGLE_UNIT()
SI_UNIT($,.RADIAN.)
);
#19622=(
NAMED_UNIT(*)
SI_UNIT($,.STERADIAN.)
SOLID_ANGLE_UNIT()
);
#19623=SHAPE_DEFINITION_REPRESENTATION(#19635,#19663);
#19624=SHAPE_DEFINITION_REPRESENTATION(#19636,#19664);
#19625=SHAPE_DEFINITION_REPRESENTATION(#19637,#19665);
#19626=SHAPE_DEFINITION_REPRESENTATION(#19638,#19666);
#19627=SHAPE_DEFINITION_REPRESENTATION(#19639,#19667);
#19628=SHAPE_DEFINITION_REPRESENTATION(#19640,#19668);
#19629=SHAPE_DEFINITION_REPRESENTATION(#19641,#19669);
#19630=SHAPE_DEFINITION_REPRESENTATION(#19642,#19670);
#19631=SHAPE_DEFINITION_REPRESENTATION(#19643,#19671);
#19632=SHAPE_DEFINITION_REPRESENTATION(#19644,#19672);
#19633=SHAPE_DEFINITION_REPRESENTATION(#19645,#19673);
#19634=SHAPE_DEFINITION_REPRESENTATION(#19654,#19674);
#19635=PRODUCT_DEFINITION_SHAPE('',$,#19676);
#19636=PRODUCT_DEFINITION_SHAPE('',$,#19677);
#19637=PRODUCT_DEFINITION_SHAPE('',$,#19678);
#19638=PRODUCT_DEFINITION_SHAPE('',$,#19679);
#19639=PRODUCT_DEFINITION_SHAPE('',$,#19680);
#19640=PRODUCT_DEFINITION_SHAPE('',$,#19681);
#19641=PRODUCT_DEFINITION_SHAPE('',$,#19682);
#19642=PRODUCT_DEFINITION_SHAPE('',$,#19683);
#19643=PRODUCT_DEFINITION_SHAPE('',$,#19684);
#19644=PRODUCT_DEFINITION_SHAPE('',$,#19685);
#19645=PRODUCT_DEFINITION_SHAPE('',$,#19686);
#19646=PRODUCT_DEFINITION_SHAPE($,$,#59);
#19647=PRODUCT_DEFINITION_SHAPE($,$,#60);
#19648=PRODUCT_DEFINITION_SHAPE($,$,#61);
#19649=PRODUCT_DEFINITION_SHAPE($,$,#62);
#19650=PRODUCT_DEFINITION_SHAPE($,$,#63);
#19651=PRODUCT_DEFINITION_SHAPE($,$,#64);
#19652=PRODUCT_DEFINITION_SHAPE($,$,#65);
#19653=PRODUCT_DEFINITION_SHAPE($,$,#66);
#19654=PRODUCT_DEFINITION_SHAPE('',$,#19687);
#19655=PRODUCT_DEFINITION_SHAPE($,$,#67);
#19656=PRODUCT_DEFINITION_SHAPE($,$,#68);
#19657=PRODUCT_DEFINITION_SHAPE($,$,#69);
#19658=PRODUCT_DEFINITION_SHAPE($,$,#70);
#19659=PRODUCT_DEFINITION_SHAPE($,$,#71);
#19660=PRODUCT_DEFINITION_SHAPE($,$,#72);
#19661=PRODUCT_DEFINITION_SHAPE($,$,#73);
#19662=PRODUCT_DEFINITION_SHAPE($,$,#74);
#19663=SHAPE_REPRESENTATION('',(#7224,#7761,#7762,#7763,#7764,#7765,#7766,
#7767,#7768),#19606);
#19664=SHAPE_REPRESENTATION('',(#7225),#19607);
#19665=SHAPE_REPRESENTATION('',(#7285),#19608);
#19666=SHAPE_REPRESENTATION('',(#7343),#19609);
#19667=SHAPE_REPRESENTATION('',(#7361),#19610);
#19668=SHAPE_REPRESENTATION('',(#7372,#7744,#7745,#7746,#7747,#7748,#7749,
#7750,#7751),#19611);
#19669=SHAPE_REPRESENTATION('',(#7373),#19612);
#19670=SHAPE_REPRESENTATION('',(#7475),#19613);
#19671=SHAPE_REPRESENTATION('',(#7583),#19614);
#19672=SHAPE_REPRESENTATION('',(#7636),#19615);
#19673=SHAPE_REPRESENTATION('',(#7718),#19616);
#19674=SHAPE_REPRESENTATION('',(#7752),#19617);
#19675=PRODUCT_DEFINITION_CONTEXT('part definition',#19713,'design');
#19676=PRODUCT_DEFINITION('TOOL-021','TOOL-021',#19688,#19675);
#19677=PRODUCT_DEFINITION('Forged jaw and handle',
'Forged jaw and handle',#19689,#19675);
#19678=PRODUCT_DEFINITION('Moving jaw and handle',
'Moving jaw and handle',#19690,#19675);
#19679=PRODUCT_DEFINITION('Shoulder pivot pin','Shoulder pivot pin',#19691,
#19675);
#19680=PRODUCT_DEFINITION('Pivot retaining ring','Pivot retaining ring',
#19692,#19675);
#19681=PRODUCT_DEFINITION('Soft grip module','Soft grip module',#19693,
#19675);
#19682=PRODUCT_DEFINITION('2026-11-10-01-34-59-955',
'Upper structural shell',#19694,#19675);
#19683=PRODUCT_DEFINITION('2026-11-10-01-34-59-959',
'Lower structural shell',#19695,#19675);
#19684=PRODUCT_DEFINITION('2026-11-10-01-34-59-964','Soft grip layer',#19696,
#19675);
#19685=PRODUCT_DEFINITION('2026-11-10-01-34-59-967',
'Socket head cap screw M3x16',#19697,#19675);
#19686=PRODUCT_DEFINITION('2026-11-10-01-34-59-968','Hex nut M3',#19698,
#19675);
#19687=PRODUCT_DEFINITION('Pivot thrust washer','Pivot thrust washer',#19699,
#19675);
#19688=PRODUCT_DEFINITION_FORMATION('',$,#19715);
#19689=PRODUCT_DEFINITION_FORMATION('',$,#19716);
#19690=PRODUCT_DEFINITION_FORMATION('',$,#19717);
#19691=PRODUCT_DEFINITION_FORMATION('',$,#19718);
#19692=PRODUCT_DEFINITION_FORMATION('',$,#19719);
#19693=PRODUCT_DEFINITION_FORMATION('',$,#19720);
#19694=PRODUCT_DEFINITION_FORMATION('',$,#19721);
#19695=PRODUCT_DEFINITION_FORMATION('',$,#19722);
#19696=PRODUCT_DEFINITION_FORMATION('',$,#19723);
#19697=PRODUCT_DEFINITION_FORMATION('',$,#19724);
#19698=PRODUCT_DEFINITION_FORMATION('',$,#19725);
#19699=PRODUCT_DEFINITION_FORMATION('',$,#19726);
#19700=PRODUCT_RELATED_PRODUCT_CATEGORY('TOOL-021','TOOL-021',(#19715));
#19701=PRODUCT_RELATED_PRODUCT_CATEGORY('Forged jaw and handle',
'Forged jaw and handle',(#19716));
#19702=PRODUCT_RELATED_PRODUCT_CATEGORY('Moving jaw and handle',
'Moving jaw and handle',(#19717));
#19703=PRODUCT_RELATED_PRODUCT_CATEGORY('Shoulder pivot pin',
'Shoulder pivot pin',(#19718));
#19704=PRODUCT_RELATED_PRODUCT_CATEGORY('Pivot retaining ring',
'Pivot retaining ring',(#19719));
#19705=PRODUCT_RELATED_PRODUCT_CATEGORY('Soft grip module',
'Soft grip module',(#19720));
#19706=PRODUCT_RELATED_PRODUCT_CATEGORY('Upper structural shell',
'Upper structural shell',(#19721));
#19707=PRODUCT_RELATED_PRODUCT_CATEGORY('Lower structural shell',
'Lower structural shell',(#19722));
#19708=PRODUCT_RELATED_PRODUCT_CATEGORY('Soft grip layer',
'Soft grip layer',(#19723));
#19709=PRODUCT_RELATED_PRODUCT_CATEGORY('Socket head cap screw M3x16',
'Socket head cap screw M3x16',(#19724));
#19710=PRODUCT_RELATED_PRODUCT_CATEGORY('Hex nut M3','Hex nut M3',(#19725));
#19711=PRODUCT_RELATED_PRODUCT_CATEGORY('Pivot thrust washer',
'Pivot thrust washer',(#19726));
#19712=APPLICATION_PROTOCOL_DEFINITION('international standard',
'automotive_design',2009,#19713);
#19713=APPLICATION_CONTEXT(
'Core Data for Automotive Mechanical Design Process');
#19714=PRODUCT_CONTEXT('part definition',#19713,'mechanical');
#19715=PRODUCT('TOOL-021','TOOL-021',$,(#19714));
#19716=PRODUCT('Forged jaw and handle','Forged jaw and handle',$,(#19714));
#19717=PRODUCT('Moving jaw and handle','Moving jaw and handle',$,(#19714));
#19718=PRODUCT('Shoulder pivot pin','Shoulder pivot pin',$,(#19714));
#19719=PRODUCT('Pivot retaining ring','Pivot retaining ring',$,(#19714));
#19720=PRODUCT('Soft grip module','Soft grip module',$,(#19714));
#19721=PRODUCT('2026-11-10-01-34-59-955','Upper structural shell',$,(#19714));
#19722=PRODUCT('2026-11-10-01-34-59-959','Lower structural shell',$,(#19714));
#19723=PRODUCT('2026-11-10-01-34-59-964','Soft grip layer',$,(#19714));
#19724=PRODUCT('2026-11-10-01-34-59-967','Socket head cap screw M3x16',
$,(#19714));
#19725=PRODUCT('2026-11-10-01-34-59-968','Hex nut M3',$,(#19714));
#19726=PRODUCT('Pivot thrust washer','Pivot thrust washer',$,(#19714));
#19727=PRESENTATION_STYLE_ASSIGNMENT((#19735));
#19728=PRESENTATION_STYLE_ASSIGNMENT((#19736));
#19729=PRESENTATION_STYLE_ASSIGNMENT((#19737));
#19730=PRESENTATION_STYLE_ASSIGNMENT((#19738));
#19731=PRESENTATION_STYLE_ASSIGNMENT((#19739));
#19732=PRESENTATION_STYLE_ASSIGNMENT((#19740));
#19733=PRESENTATION_STYLE_ASSIGNMENT((#19741));
#19734=PRESENTATION_STYLE_ASSIGNMENT((#19742));
#19735=SURFACE_STYLE_USAGE(.BOTH.,#19743);
#19736=SURFACE_STYLE_USAGE(.BOTH.,#19744);
#19737=SURFACE_STYLE_USAGE(.BOTH.,#19745);
#19738=SURFACE_STYLE_USAGE(.BOTH.,#19746);
#19739=SURFACE_STYLE_USAGE(.BOTH.,#19747);
#19740=SURFACE_STYLE_USAGE(.BOTH.,#19748);
#19741=SURFACE_STYLE_USAGE(.BOTH.,#19749);
#19742=SURFACE_STYLE_USAGE(.BOTH.,#19750);
#19743=SURFACE_SIDE_STYLE('',(#19751));
#19744=SURFACE_SIDE_STYLE('',(#19752));
#19745=SURFACE_SIDE_STYLE('',(#19753));
#19746=SURFACE_SIDE_STYLE('',(#19754));
#19747=SURFACE_SIDE_STYLE('',(#19755));
#19748=SURFACE_SIDE_STYLE('',(#19756));
#19749=SURFACE_SIDE_STYLE('',(#19757));
#19750=SURFACE_SIDE_STYLE('',(#19758));
#19751=SURFACE_STYLE_FILL_AREA(#19759);
#19752=SURFACE_STYLE_FILL_AREA(#19760);
#19753=SURFACE_STYLE_FILL_AREA(#19761);
#19754=SURFACE_STYLE_FILL_AREA(#19762);
#19755=SURFACE_STYLE_FILL_AREA(#19763);
#19756=SURFACE_STYLE_FILL_AREA(#19764);
#19757=SURFACE_STYLE_FILL_AREA(#19765);
#19758=SURFACE_STYLE_FILL_AREA(#19766);
#19759=FILL_AREA_STYLE('Steel - Satin',(#19767));
#19760=FILL_AREA_STYLE('Tool steel gray',(#19768));
#19761=FILL_AREA_STYLE('Pivot dark gray',(#19769));
#19762=FILL_AREA_STYLE('Dark gray',(#19770));
#19763=FILL_AREA_STYLE('Structural dark blue',(#19771));
#19764=FILL_AREA_STYLE('Sky blue soft grip',(#19772));
#19765=FILL_AREA_STYLE('Fastener gray',(#19773));
#19766=FILL_AREA_STYLE('Washer gray',(#19774));
#19767=FILL_AREA_STYLE_COLOUR('Steel - Satin',#19775);
#19768=FILL_AREA_STYLE_COLOUR('Tool steel gray',#19776);
#19769=FILL_AREA_STYLE_COLOUR('Pivot dark gray',#19777);
#19770=FILL_AREA_STYLE_COLOUR('Dark gray',#19778);
#19771=FILL_AREA_STYLE_COLOUR('Structural dark blue',#19779);
#19772=FILL_AREA_STYLE_COLOUR('Sky blue soft grip',#19780);
#19773=FILL_AREA_STYLE_COLOUR('Fastener gray',#19781);
#19774=FILL_AREA_STYLE_COLOUR('Washer gray',#19782);
#19775=COLOUR_RGB('Steel - Satin',0.627450980392157,0.627450980392157,0.627450980392157);
#19776=COLOUR_RGB('Tool steel gray',0.607843137254902,0.643137254901961,
0.698039215686274);
#19777=COLOUR_RGB('Pivot dark gray',0.27843137254902,0.309803921568627,
0.352941176470588);
#19778=COLOUR_RGB('Dark gray',0.250980392156863,0.282352941176471,0.32156862745098);
#19779=COLOUR_RGB('Structural dark blue',0.0901960784313725,0.270588235294118,
0.513725490196078);
#19780=COLOUR_RGB('Sky blue soft grip',0.27843137254902,0.309803921568627,
0.352941176470588);
#19781=COLOUR_RGB('Fastener gray',0.607843137254902,0.643137254901961,0.698039215686274);
#19782=COLOUR_RGB('Washer gray',0.725490196078431,0.752941176470588,0.792156862745098);
ENDSEC;
END-ISO-10303-21;
